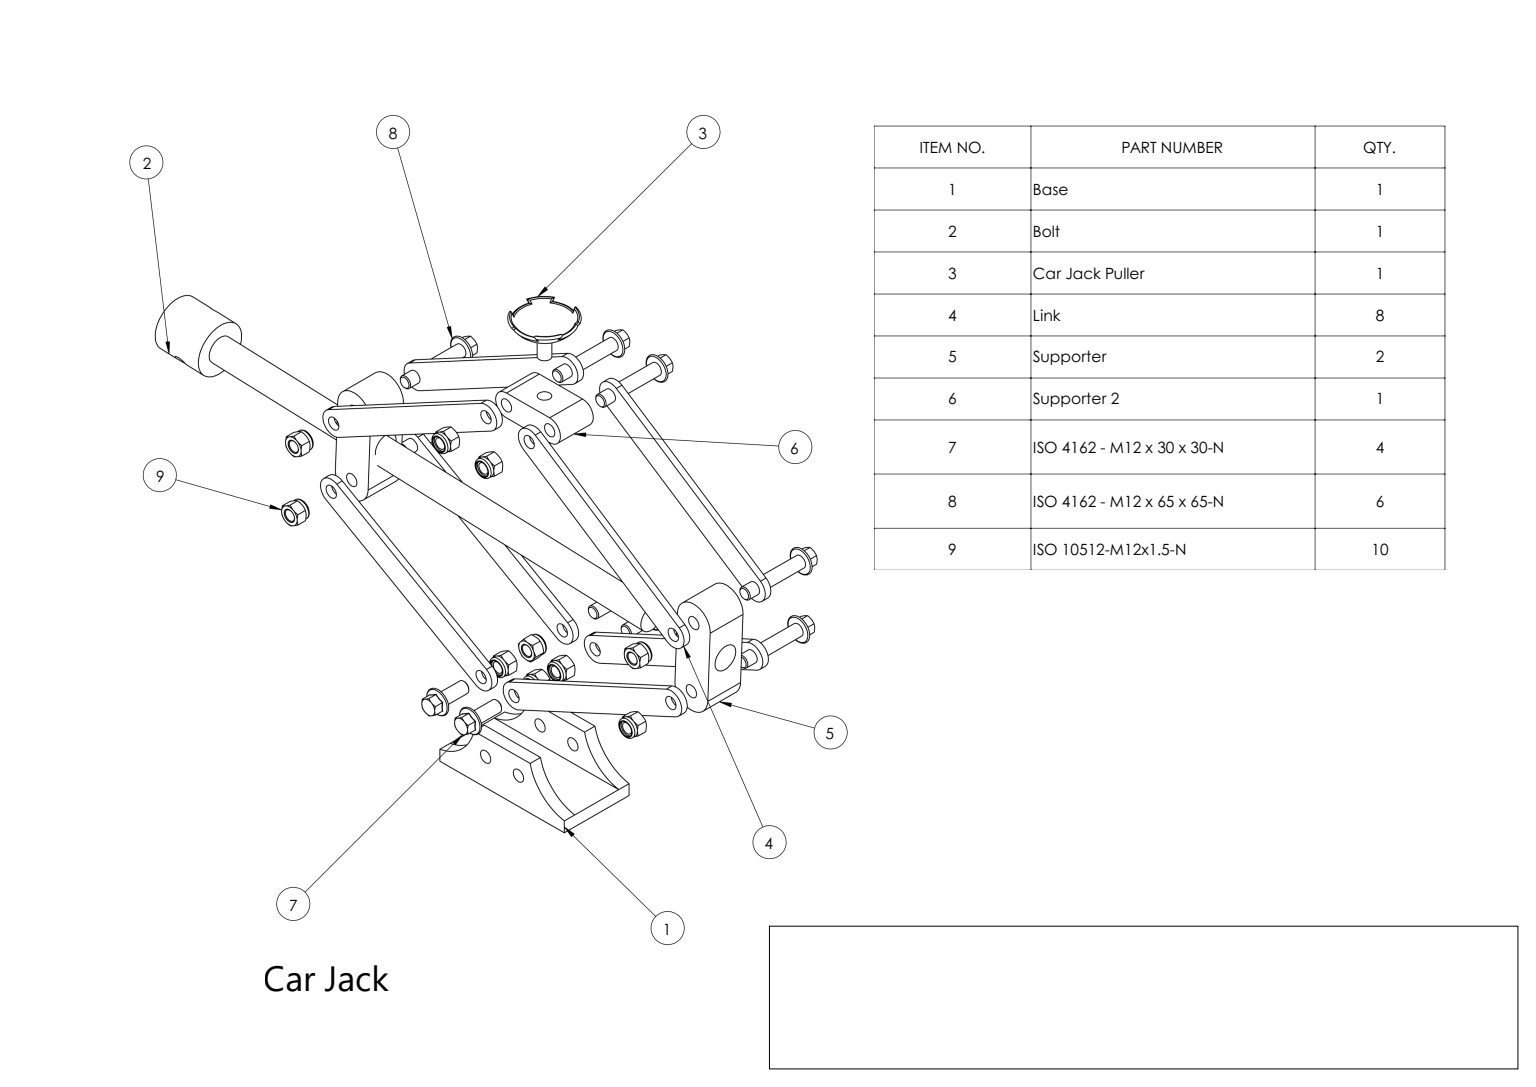
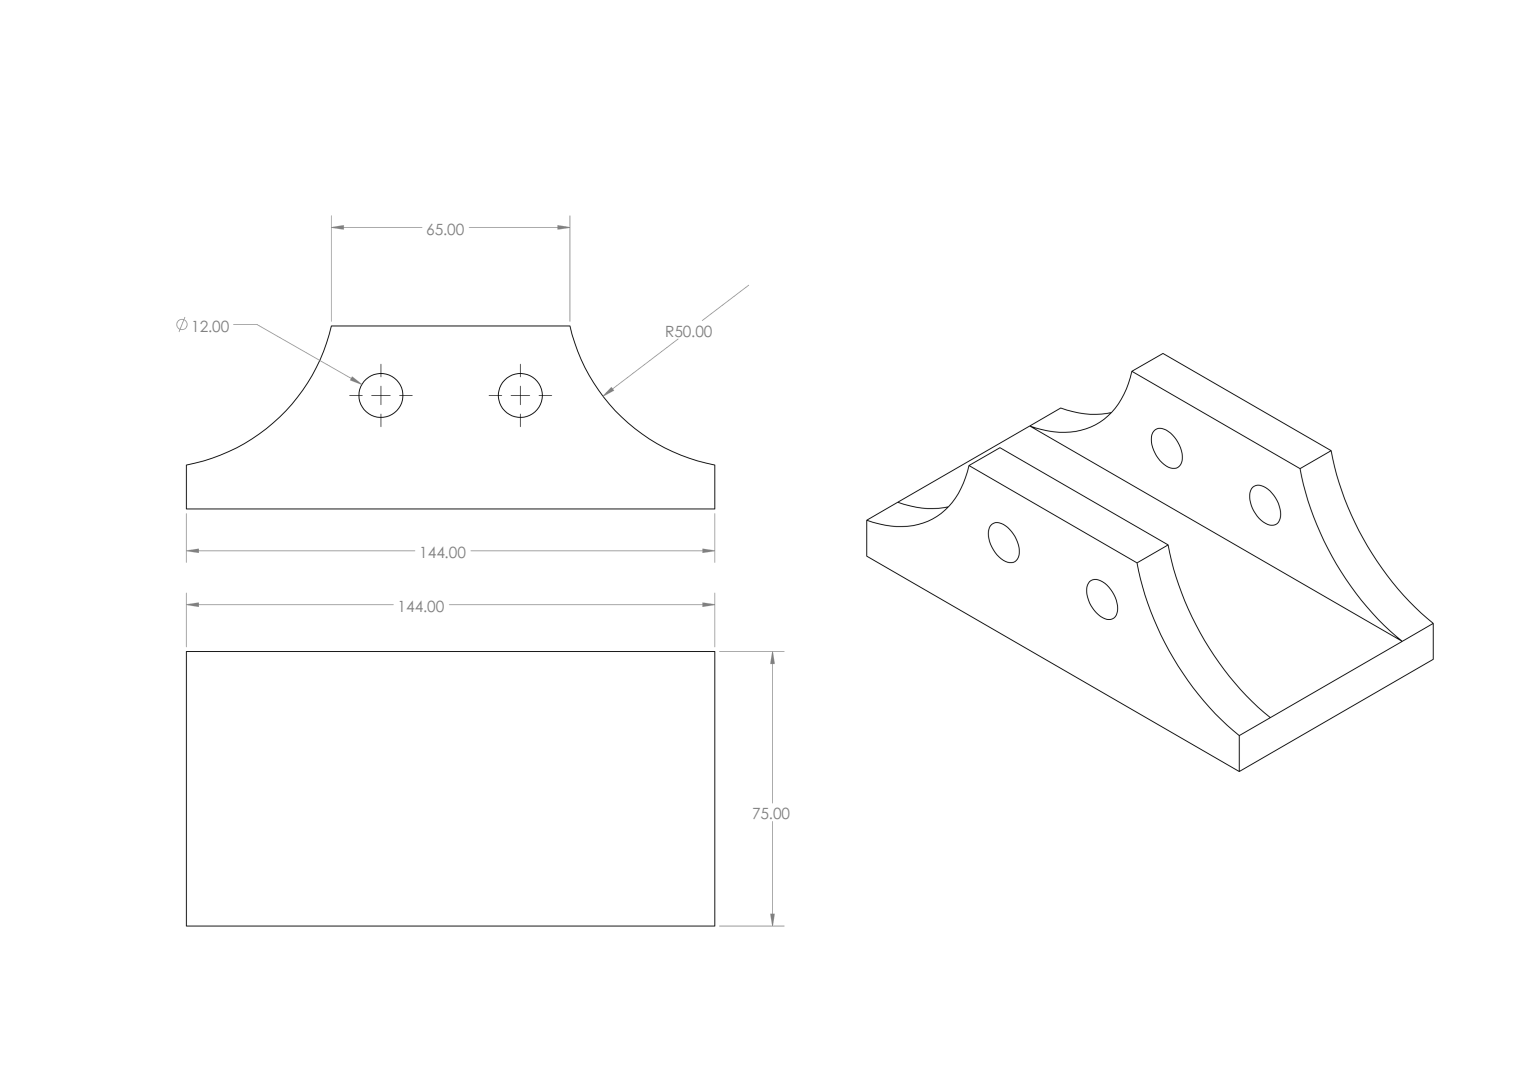
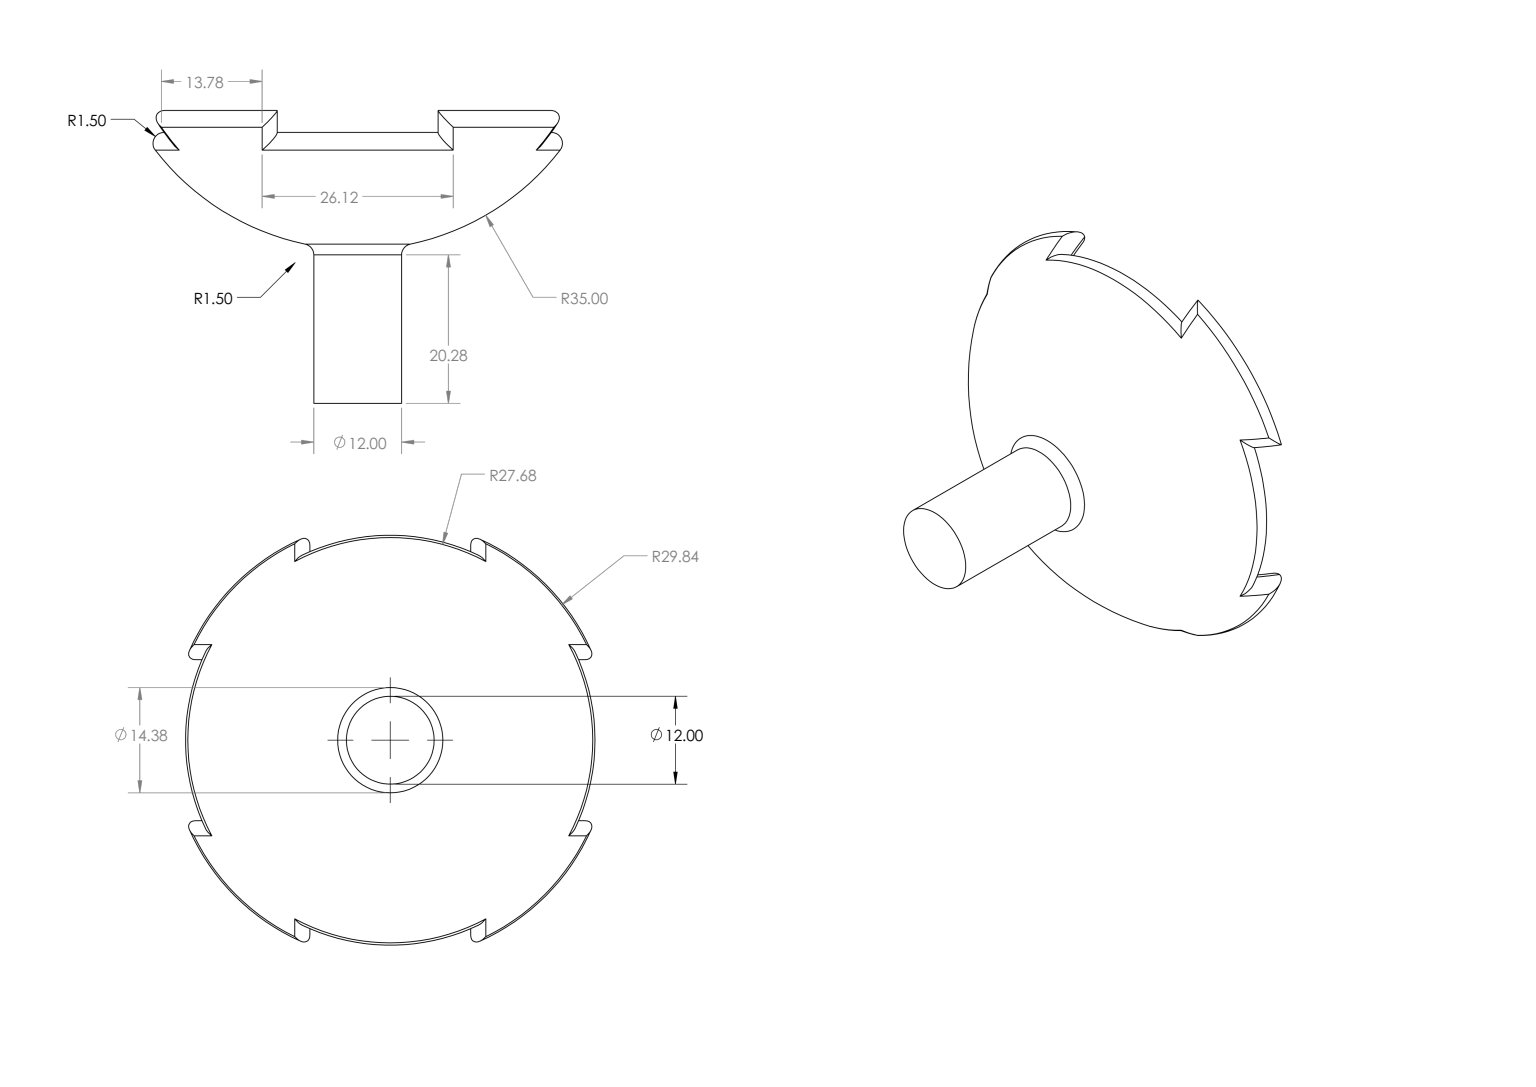
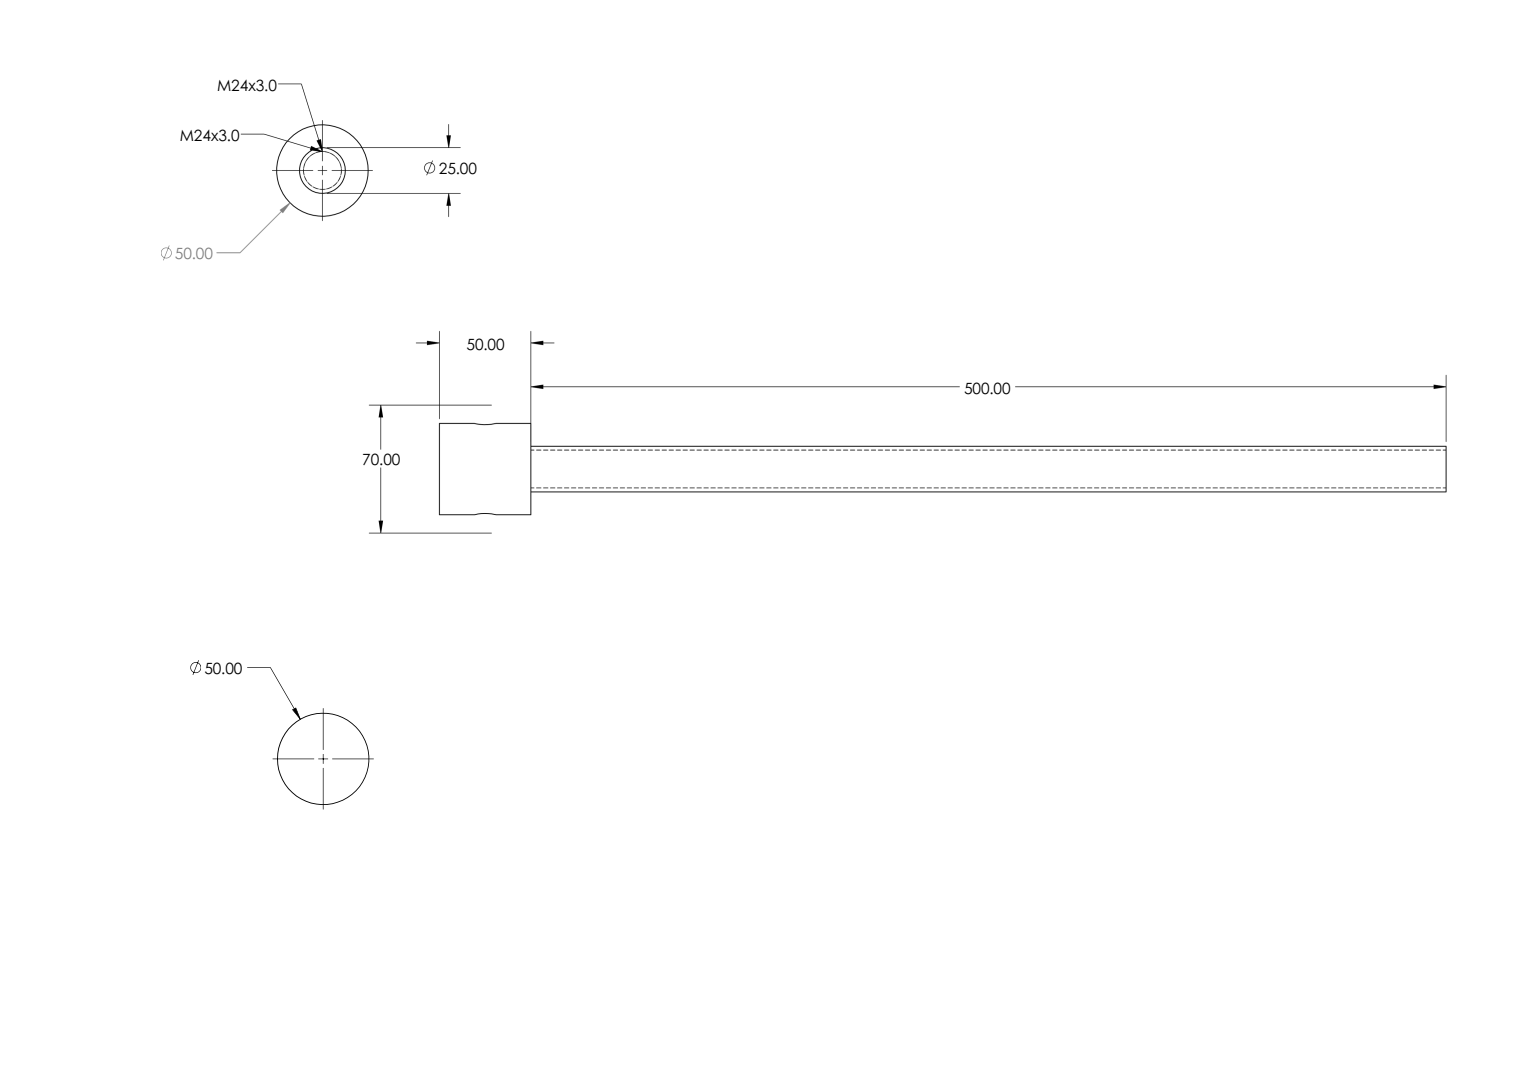
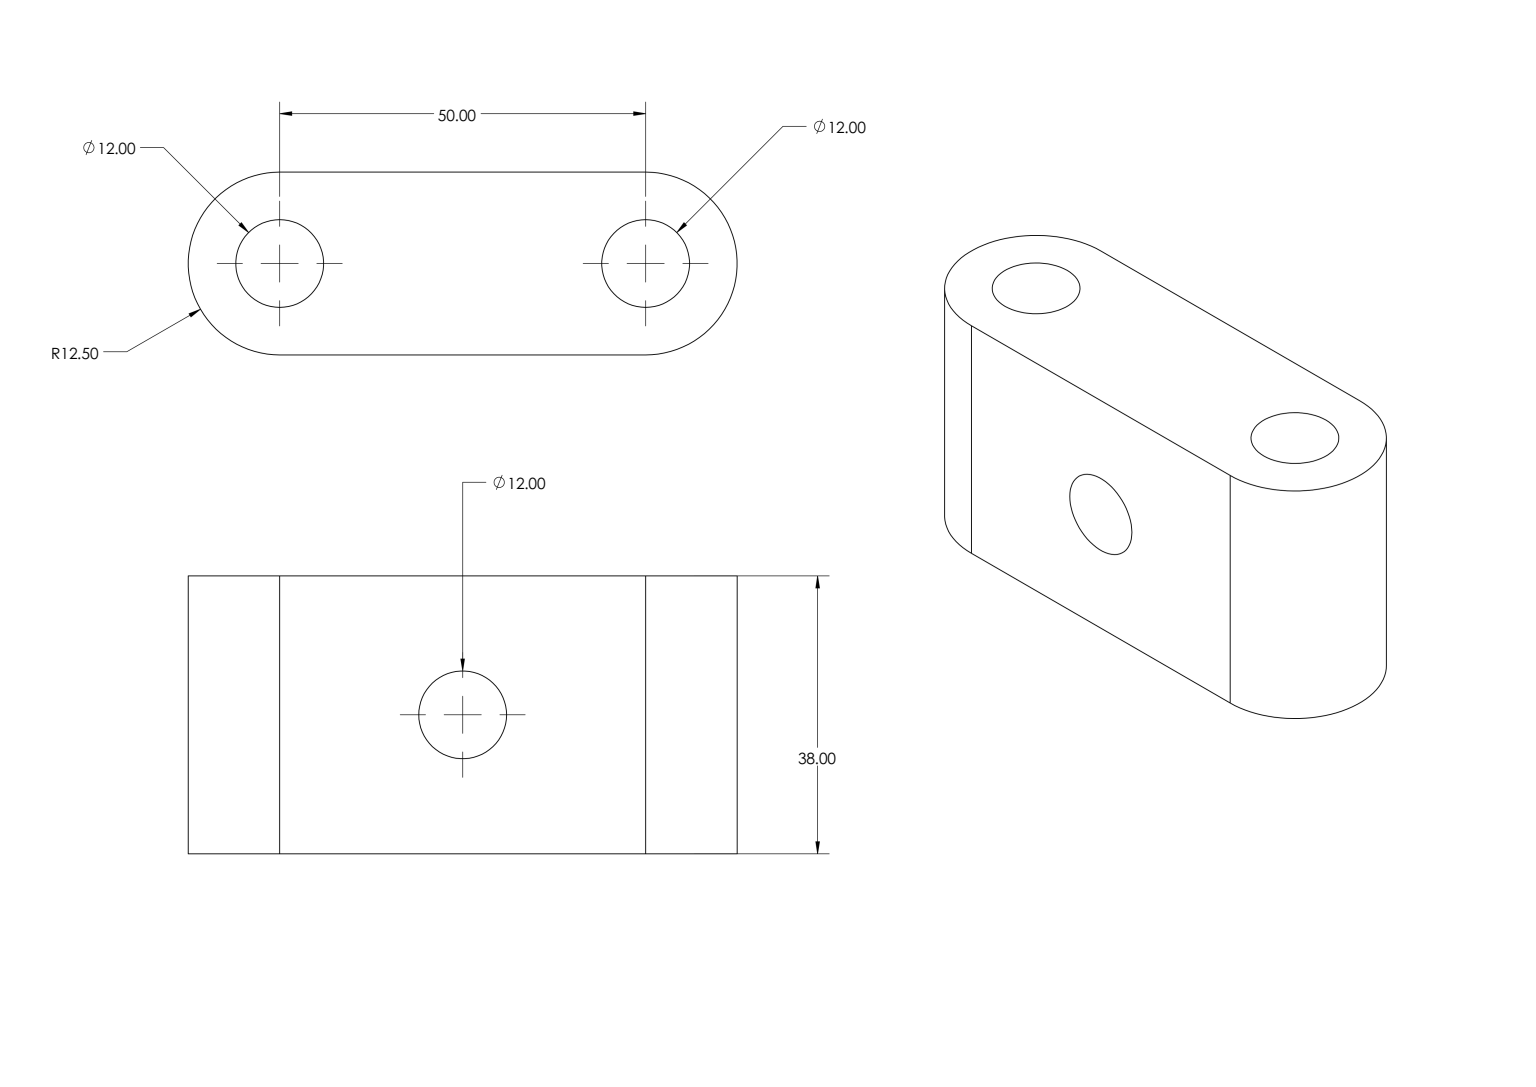
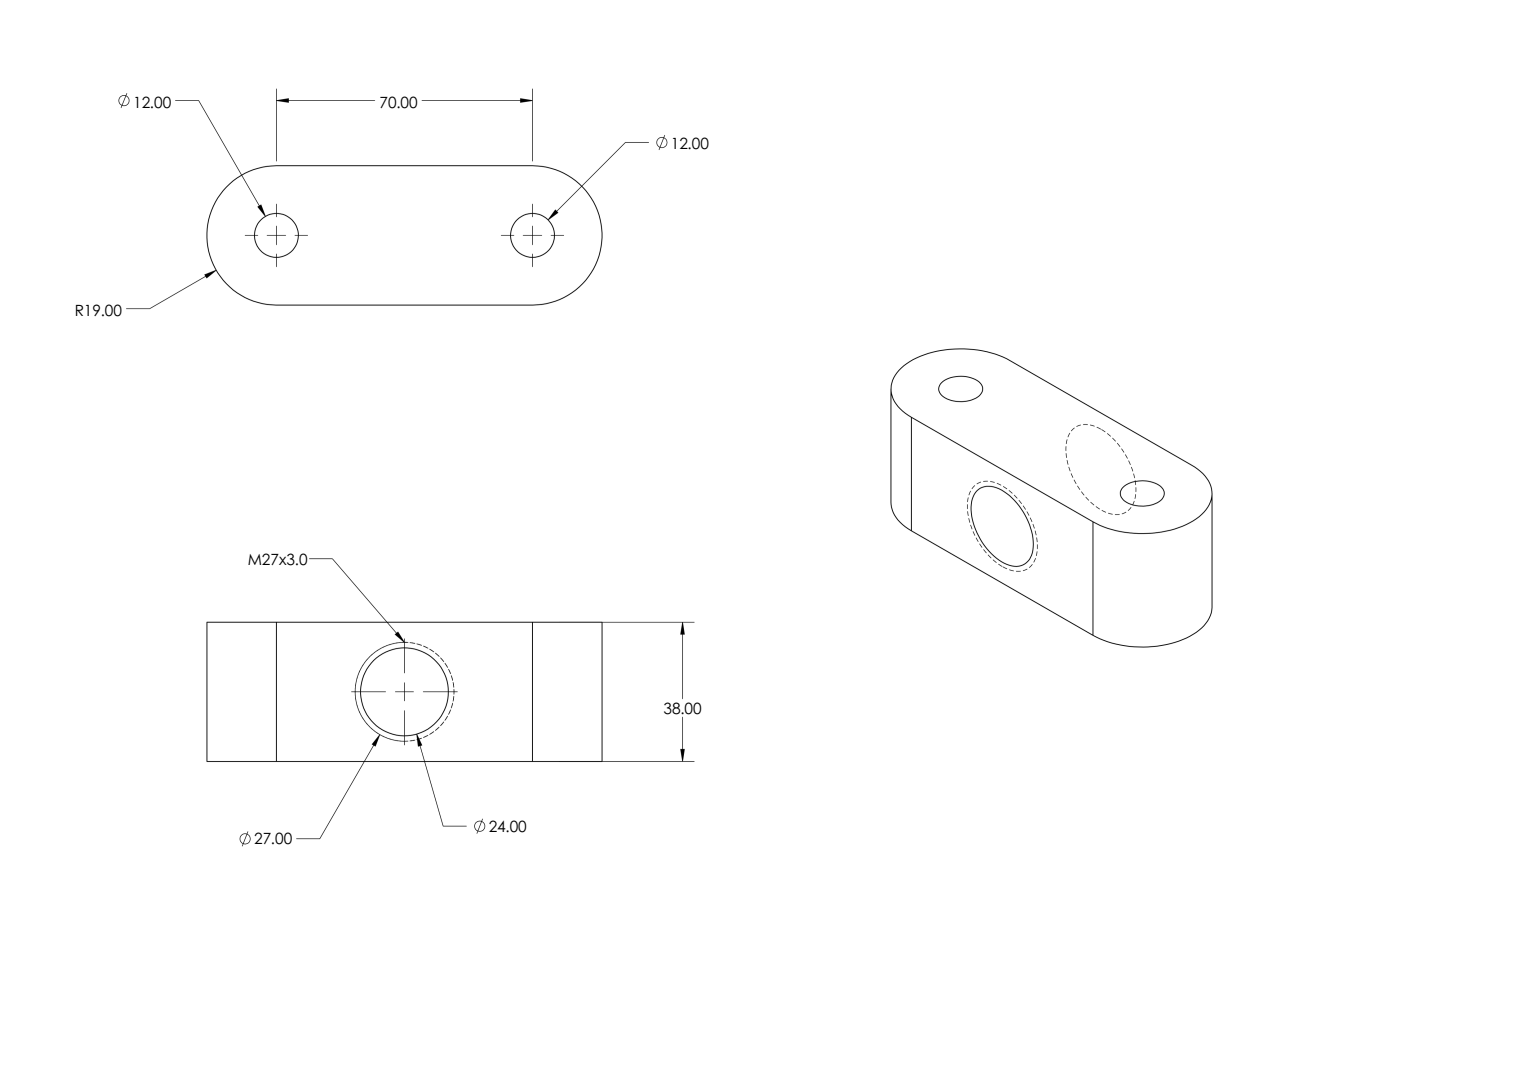
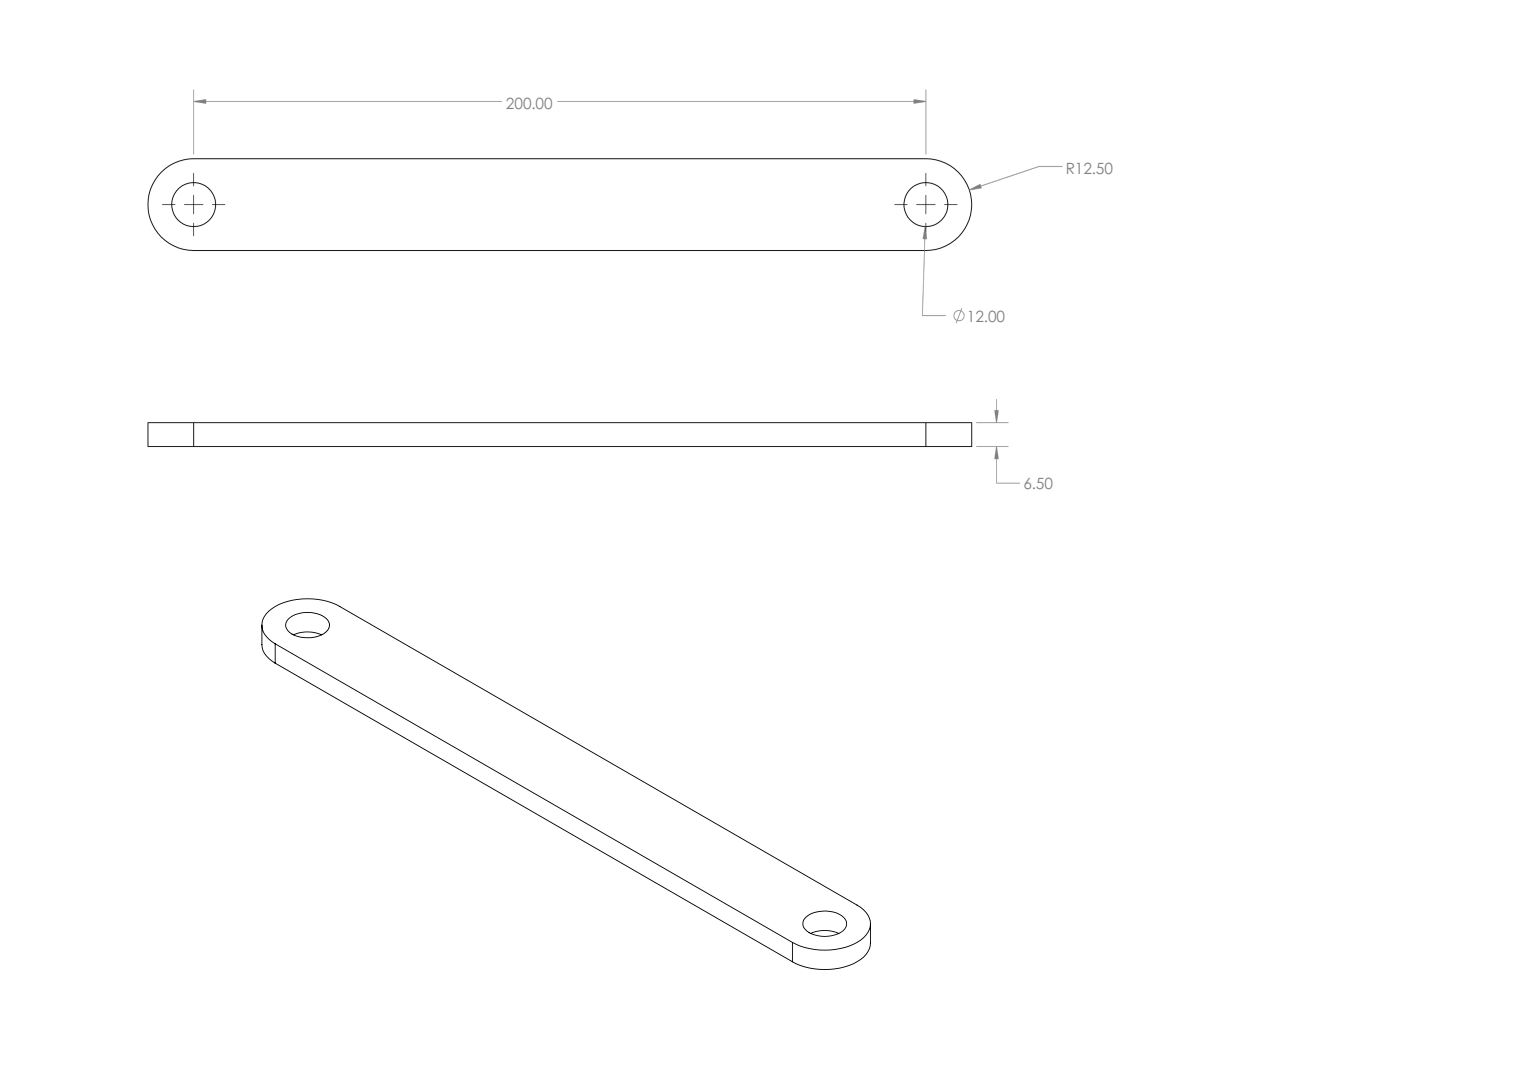
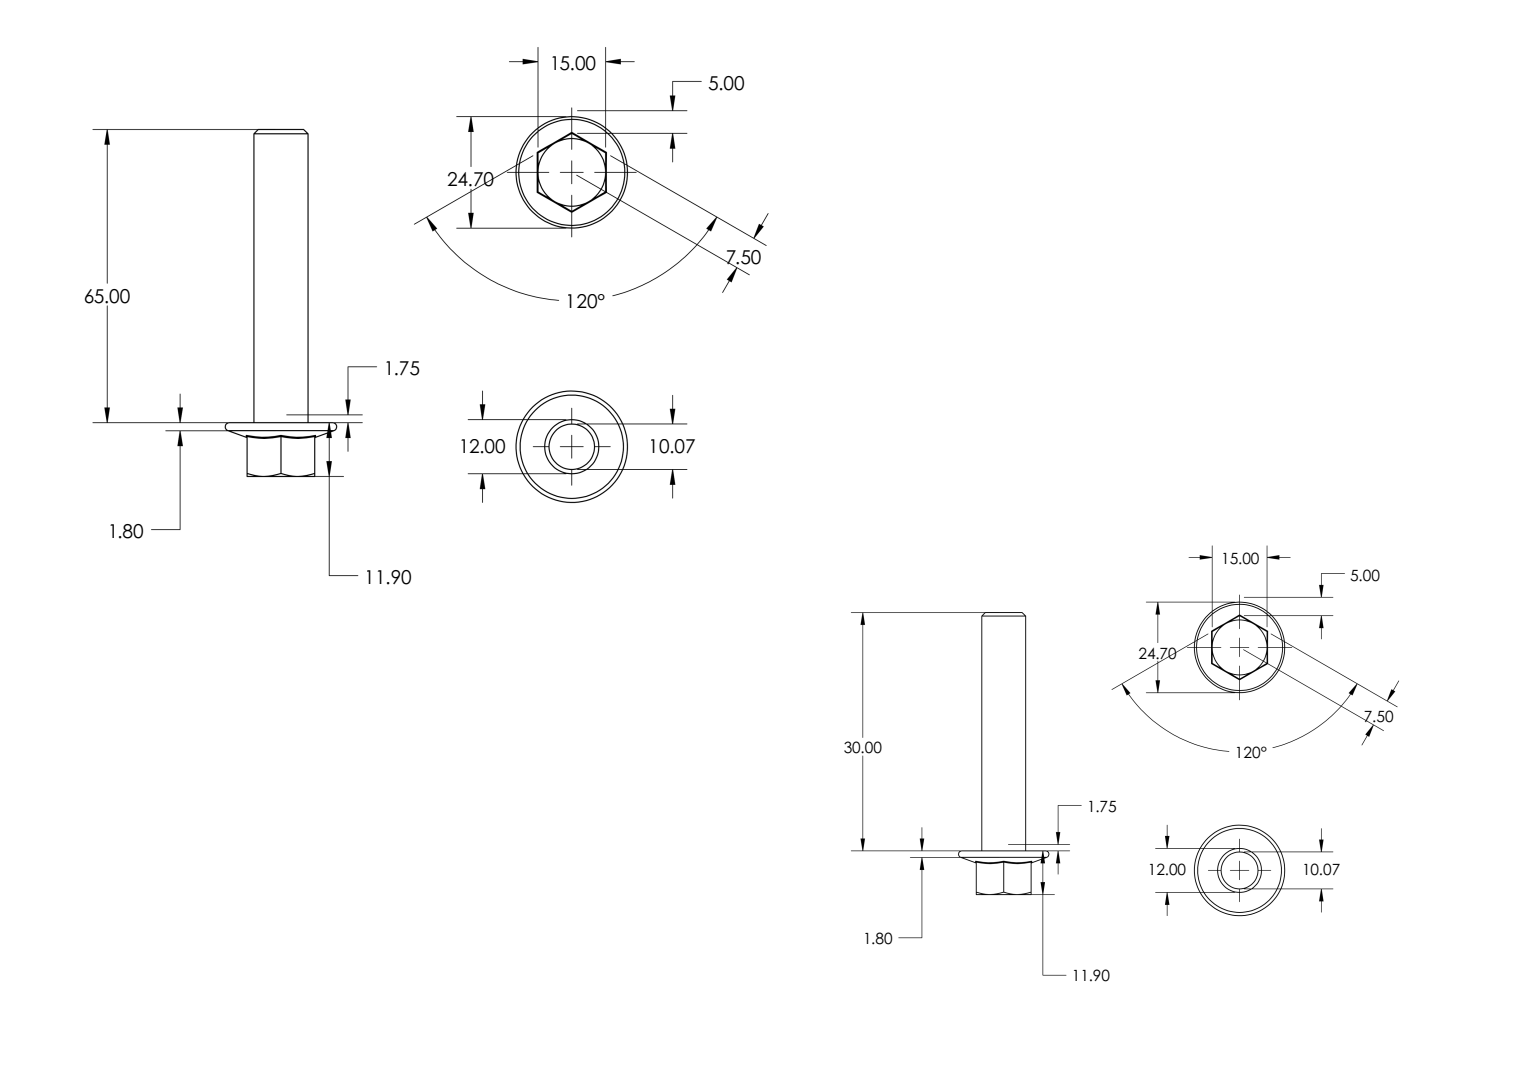
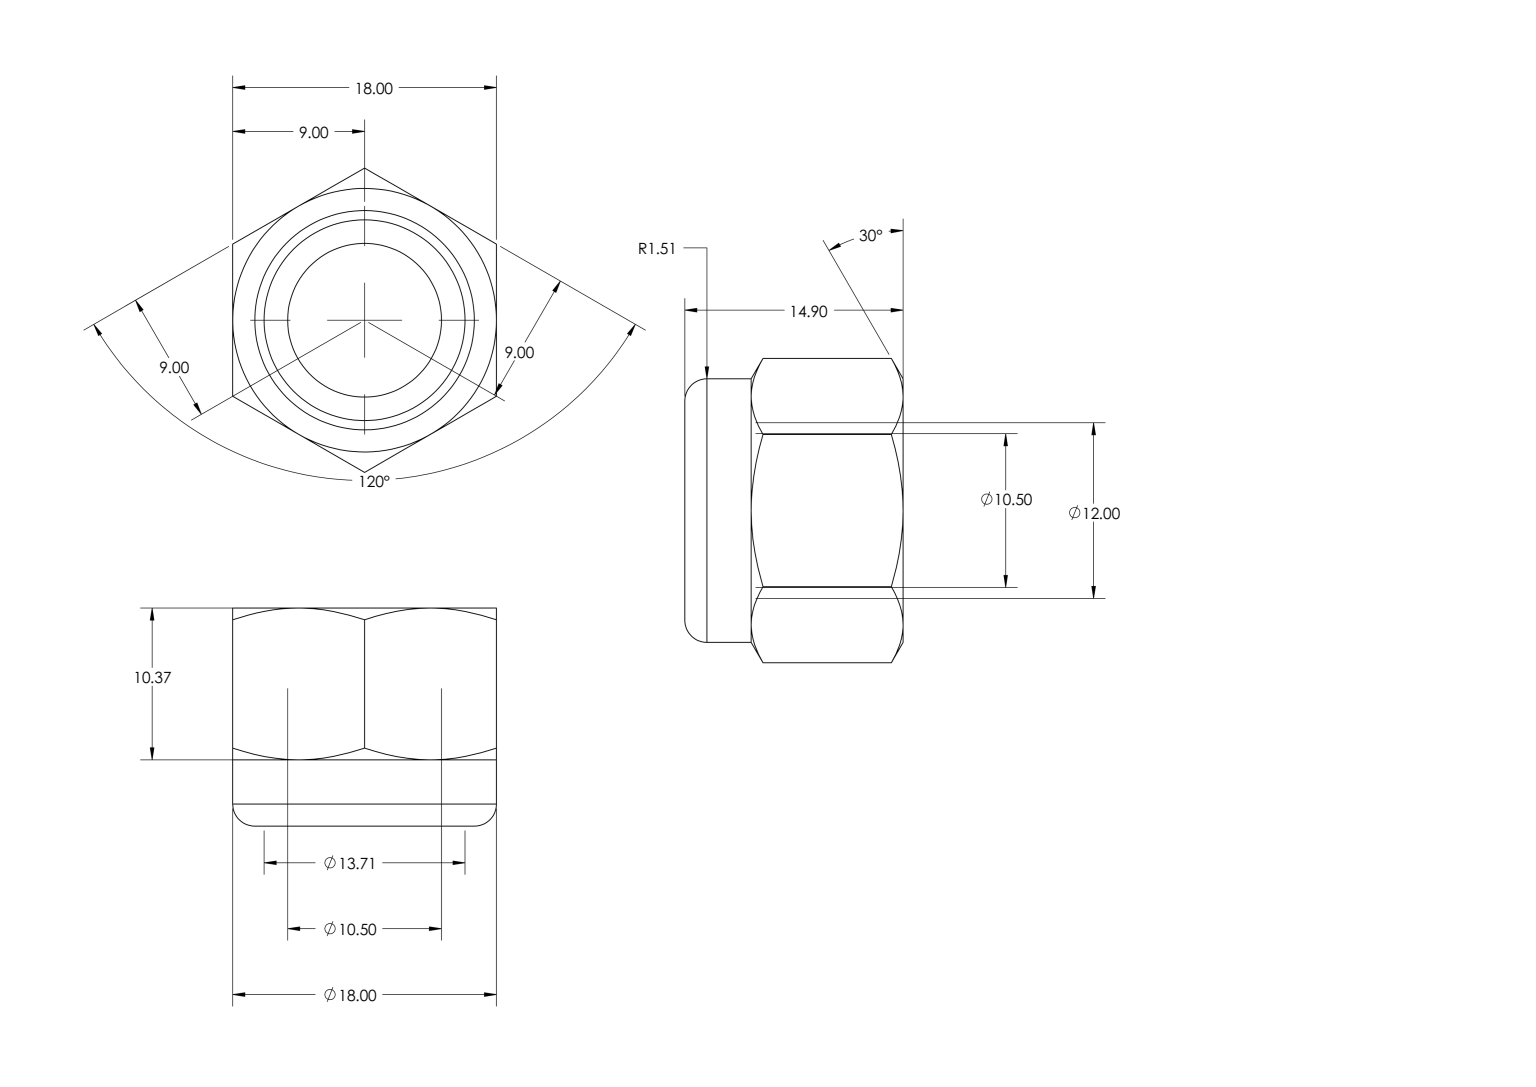
ISO-10303-21;
HEADER;
FILE_DESCRIPTION (('STEP AP214'),
    '1' );
FILE_NAME ('MAT-019',
    '2026-10-23T20:35:44',
    ( '' ),
    ( '' ),
    'SwSTEP 2.0',
    'SolidWorks 2025',
    '' );
FILE_SCHEMA (( 'AUTOMOTIVE_DESIGN' ));
ENDSEC;

DATA;
#1 = VERTEX_POINT ( 'NONE', #349 ) ;
#2 = CARTESIAN_POINT ( 'NONE',  ( 1.172031980416358365, -0.1441408498666779114, 0.9737261629585141076 ) ) ;
#3 = EDGE_CURVE ( 'NONE', #4293, #4703, #7002, .T. ) ;
#4 = CARTESIAN_POINT ( 'NONE',  ( 0.3581828924050324825, 0.3486337532542225226, 1.056976728655274672E-17 ) ) ;
#5 = ORIENTED_EDGE ( 'NONE', *, *, #5535, .F. ) ;
#6 = CARTESIAN_POINT ( 'NONE',  ( -0.3543307086614173596, -0.1713008003332314455, -0.02204270589528184790 ) ) ;
#7 = CIRCLE ( 'NONE', #3434, 0.2362204724409449064 ) ;
#8 = CARTESIAN_POINT ( 'NONE',  ( -1.023371766162646468, 0.4368380215374090825, -1.573834103987475475 ) ) ;
#9 = ADVANCED_FACE ( 'NONE', ( #4327 ), #5594, .T. ) ;
#10 = VERTEX_POINT ( 'NONE', #4360 ) ;
#11 = DIRECTION ( 'NONE',  ( -0.000000000000000000, -0.000000000000000000, 1.000000000000000000 ) ) ;
#12 = CARTESIAN_POINT ( 'NONE',  ( 0.3321019207957557895, 0.02907045490630093265, 0.2952755905511811330 ) ) ;
#13 = DIRECTION ( 'NONE',  ( -0.9237280213470682178, -0.3830490080632377725, 0.000000000000000000 ) ) ;
#14 = CIRCLE ( 'NONE', #4286, 0.4629062255509093782 ) ;
#15 =( NAMED_UNIT ( * ) PLANE_ANGLE_UNIT ( ) SI_UNIT ( $, .RADIAN. ) );
#16 = CARTESIAN_POINT ( 'NONE',  ( -0.4330708661417322913, -0.9666437042230143772, -1.454455828411337359 ) ) ;
#17 = CARTESIAN_POINT ( 'NONE',  ( 0.4330708661417324024, 0.000000000000000000, 0.000000000000000000 ) ) ;
#18 = VERTEX_POINT ( 'NONE', #5013 ) ;
#19 = FACE_OUTER_BOUND ( 'NONE', #4746, .T. ) ;
#20 = AXIS2_PLACEMENT_3D ( 'NONE', #1580, #1013, #4418 ) ;
#21 = ORIENTED_EDGE ( 'NONE', *, *, #1765, .T. ) ;
#22 = CIRCLE ( 'NONE', #2939, 0.4921259842519685179 ) ;
#23 = SHAPE_REPRESENTATION_RELATIONSHIP ( 'NONE' , 'NONE' ,  #2912, #3774 ) ;
#24 = CIRCLE ( 'NONE', #5042, 0.2362204724409449619 ) ;
#25 = DIRECTION ( 'NONE',  ( 0.000000000000000000, 0.000000000000000000, -1.000000000000000000 ) ) ;
#26 = TOROIDAL_SURFACE ( 'NONE', #1116, 1.223643328182681289, 0.05905511811023622659 ) ;
#27 = DIRECTION ( 'NONE',  ( -0.000000000000000000, 1.000000000000000000, 0.000000000000000000 ) ) ;
#28 = AXIS2_PLACEMENT_3D ( 'NONE', #7517, #513, #2824 ) ;
#29 =( REPRESENTATION_RELATIONSHIP ('NONE','NONE', #303, #1552 ) REPRESENTATION_RELATIONSHIP_WITH_TRANSFORMATION ( #2886 )SHAPE_REPRESENTATION_RELATIONSHIP( ) );
#30 = CARTESIAN_POINT ( 'NONE',  ( 0.3527008206095850751, 0.1709223649093223329, 0.2960462201727743214 ) ) ;
#31 = CARTESIAN_POINT ( 'NONE',  ( 0.3543307086614173596, -0.2045729300278204543, -0.03164754241312491001 ) ) ;
#32 = CARTESIAN_POINT ( 'NONE',  ( 0.000000000000000000, -0.2557161625347750822, -0.1476377952755907330 ) ) ;
#33 = CARTESIAN_POINT ( 'NONE',  ( -0.4330708661417322913, 0.9666437042230143772, -1.454455828411337359 ) ) ;
#34 = VERTEX_POINT ( 'NONE', #3752 ) ;
#35 = CIRCLE ( 'NONE', #6758, 1.377952755905511806 ) ;
#36 = CARTESIAN_POINT ( 'NONE',  ( -0.4330708661417317917, -1.051607547633158557, -1.573502280244650997 ) ) ;
#37 = ORIENTED_EDGE ( 'NONE', *, *, #488, .F. ) ;
#38 = CARTESIAN_POINT ( 'NONE',  ( 0.8794895096619267383, -0.2118599820681134061, 0.9611874069187010816 ) ) ;
#39 = ADVANCED_FACE ( 'NONE', ( #5518 ), #2011, .T. ) ;
#40 = DIRECTION ( 'NONE',  ( 1.000000000000000000, 0.000000000000000000, 0.000000000000000000 ) ) ;
#41 = ORIENTED_EDGE ( 'NONE', *, *, #1877, .F. ) ;
#42 = CARTESIAN_POINT ( 'NONE',  ( 0.4637694296357178780, 0.9984400756355444884, -1.410742812766313969 ) ) ;
#43 = DIRECTION ( 'NONE',  ( 1.000000000000000000, 0.000000000000000000, 0.000000000000000000 ) ) ;
#44 = ORIENTED_EDGE ( 'NONE', *, *, #3935, .F. ) ;
#45 = VECTOR ( 'NONE', #7259, 39.37007874015748143 ) ;
#46 = CARTESIAN_POINT ( 'NONE',  ( 0.000000000000000000, 2.957312202238506242E-17, 0.2952755905511810774 ) ) ;
#47 = CARTESIAN_POINT ( 'NONE',  ( -4.923936545553797639E-15, 0.4700904924197870649, -2.204724409448822975 ) ) ;
#48 = SHAPE_DEFINITION_REPRESENTATION ( #1283, #303 ) ;
#49 = EDGE_CURVE ( 'NONE', #4478, #2222, #5824, .T. ) ;
#50 = PRESENTATION_STYLE_ASSIGNMENT (( #4751 ) ) ;
#51 = EDGE_CURVE ( 'NONE', #5178, #931, #7181, .T. ) ;
#52 = DIRECTION ( 'NONE',  ( -1.000000000000000000, -0.000000000000000000, -0.000000000000000000 ) ) ;
#53 = TOROIDAL_SURFACE ( 'NONE', #1389, 1.223643328182681289, 0.05905511811023622659 ) ;
#54 = CARTESIAN_POINT ( 'NONE',  ( -1.051607547633157225, -0.4330708661417354555, -1.573502280244651441 ) ) ;
#55 = CARTESIAN_POINT ( 'NONE',  ( 0.3336175750056032396, 0.2841290694830835850, -0.09842519685039363697 ) ) ;
#56 = ORIENTED_EDGE ( 'NONE', *, *, #571, .F. ) ;
#57 = LENGTH_MEASURE_WITH_UNIT ( LENGTH_MEASURE( 0.02539999999999999897 ), #5956 );
#58 = CARTESIAN_POINT ( 'NONE',  ( 0.9346848099469073912, -0.4388997119412443304, -1.455943619906241215 ) ) ;
#59 = CARTESIAN_POINT ( 'NONE',  ( 0.000000000000000000, 0.000000000000000000, -1.515748031496062964 ) ) ;
#60 = CARTESIAN_POINT ( 'NONE',  ( 0.000000000000000000, 1.496062992125984259, -0.2362204724409449341 ) ) ;
#61 = CARTESIAN_POINT ( 'NONE',  ( 2.892866454678787531E-17, 0.000000000000000000, 0.2362204724409449341 ) ) ;
#62 = CARTESIAN_POINT ( 'NONE',  ( 0.000000000000000000, 0.000000000000000000, 0.000000000000000000 ) ) ;
#63 = PRODUCT_DEFINITION_CONTEXT ( 'detailed design', #3952, 'design' ) ;
#64 = DIRECTION ( 'NONE',  ( 0.000000000000000000, 1.000000000000000000, 0.000000000000000000 ) ) ;
#65 = CARTESIAN_POINT ( 'NONE',  ( -0.5073702590888615749, 0.9696319393318632018, -1.367288630523146420 ) ) ;
#66 = PLANE ( 'NONE',  #3064 ) ;
#67 = CARTESIAN_POINT ( 'NONE',  ( 1.048552902599916292, 0.4330708661417427274, -1.573978973432617279 ) ) ;
#68 = PLANE ( 'NONE',  #1789 ) ;
#69 = CARTESIAN_POINT ( 'NONE',  ( 0.01841426102874288775, 0.1429077274040485568, 0.2952755905511811330 ) ) ;
#70 = DIRECTION ( 'NONE',  ( -0.000000000000000000, -1.000000000000000000, -0.000000000000000000 ) ) ;
#71 = ORIENTED_EDGE ( 'NONE', *, *, #7518, .T. ) ;
#72 = PRODUCT_DEFINITION_SHAPE ( 'NONE', 'NONE',  #5982 ) ;
#73 = CARTESIAN_POINT ( 'NONE',  ( -0.4348450093584657061, -1.063161251382699124, -1.569784523562343992 ) ) ;
#74 = CARTESIAN_POINT ( 'NONE',  ( 0.3528971332113848836, -0.3341112492250008503, 0.02492269209175877395 ) ) ;
#75 = VERTEX_POINT ( 'NONE', #2557 ) ;
#76 = ORIENTED_EDGE ( 'NONE', *, *, #2854, .T. ) ;
#77 = CARTESIAN_POINT ( 'NONE',  ( 0.3581828924050323715, 0.1743168766271109560, 0.3019256869348722616 ) ) ;
#78 = AXIS2_PLACEMENT_3D ( 'NONE', #5698, #7313, #7465 ) ;
#79 = DIRECTION ( 'NONE',  ( -1.000000000000000000, -0.000000000000000000, -0.000000000000000000 ) ) ;
#80 = ORIENTED_EDGE ( 'NONE', *, *, #4669, .F. ) ;
#81 = CARTESIAN_POINT ( 'NONE',  ( 0.4999746636856467474, 0.9773775067402665773, -1.373988502838978665 ) ) ;
#82 = ORIENTED_EDGE ( 'NONE', *, *, #3467, .F. ) ;
#83 = EDGE_CURVE ( 'NONE', #5632, #7112, #5799, .T. ) ;
#84 = CYLINDRICAL_SURFACE ( 'NONE', #4175, 0.2362204724409449341 ) ;
#85 = CARTESIAN_POINT ( 'NONE',  ( 0.3337350301074833991, 0.05917206666036364110, 0.2952755905511810774 ) ) ;
#86 = CARTESIAN_POINT ( 'NONE',  ( 0.000000000000000000, 0.000000000000000000, 0.000000000000000000 ) ) ;
#87 = B_SPLINE_CURVE_WITH_KNOTS ( 'NONE', 3,
 ( #5029, #2125, #4375, #2046, #3150, #6743, #5497, #6139, #1530 ),
 .UNSPECIFIED., .F., .F.,
 ( 4, 2, 1, 2, 4 ),
 ( 0.000000000000000000, 0.002165063509461097064, 0.004330127018922194128, 0.006495190528383291625, 0.008660254037844388256 ),
 .UNSPECIFIED. ) ;
#88 = CARTESIAN_POINT ( 'NONE',  ( 0.000000000000000000, 0.000000000000000000, -0.4082677165354330340 ) ) ;
#89 = EDGE_LOOP ( 'NONE', ( #2667, #4029, #6739, #4168 ) ) ;
#90 = VECTOR ( 'NONE', #7074, 39.37007874015748143 ) ;
#91 = LINE ( 'NONE', #2420, #7062 ) ;
#92 = ORIENTED_EDGE ( 'NONE', *, *, #6917, .F. ) ;
#93 = FACE_OUTER_BOUND ( 'NONE', #3298, .T. ) ;
#94 = B_SPLINE_CURVE_WITH_KNOTS ( 'NONE', 3,
 ( #4855, #1250, #5355, #240, #5937, #4783, #5402, #7182 ),
 .UNSPECIFIED., .F., .F.,
 ( 4, 2, 2, 4 ),
 ( 0.005257893453559878486, 0.006567392922673220834, 0.007876892391786563183, 0.01049589133001324615 ),
 .UNSPECIFIED. ) ;
#95 = EDGE_CURVE ( 'NONE', #3796, #3264, #4939, .T. ) ;
#96 = VERTEX_POINT ( 'NONE', #2710 ) ;
#97 = EDGE_CURVE ( 'NONE', #6349, #6629, #5465, .T. ) ;
#98 = AXIS2_PLACEMENT_3D ( 'NONE', #2181, #4591, #4516 ) ;
#99 = EDGE_CURVE ( 'NONE', #6172, #3346, #1437, .T. ) ;
#100 = CARTESIAN_POINT ( 'NONE',  ( -0.4437902010346558290, 0.9221077491748241872, -1.453484313640523107 ) ) ;
#101 = CARTESIAN_POINT ( 'NONE',  ( 2.755905511811024056, 1.496062992125984259, -0.7480314960629921295 ) ) ;
#102 = DIRECTION ( 'NONE',  ( -1.000000000000000000, 0.000000000000000000, 0.000000000000000000 ) ) ;
#103 = VECTOR ( 'NONE', #1652, 39.37007874015748143 ) ;
#104 = CARTESIAN_POINT ( 'NONE',  ( 0.3411144883932946681, 0.06120045565151401717, -0.3014953316451452481 ) ) ;
#105 = FACE_BOUND ( 'NONE', #1838, .T. ) ;
#106 = CARTESIAN_POINT ( 'NONE',  ( -0.4349192958999751890, 0.9810556462971158354, -1.448591228719268820 ) ) ;
#107 = CARTESIAN_POINT ( 'NONE',  ( 1.649606299212598381, 0.000000000000000000, 0.000000000000000000 ) ) ;
#108 = AXIS2_PLACEMENT_3D ( 'NONE', #6313, #3367, #512 ) ;
#109 = ITEM_DEFINED_TRANSFORMATION ( 'NONE', 'NONE', #1772,  #5166 ) ;
#110 = DIRECTION ( 'NONE',  ( -1.000000000000000000, 0.000000000000000000, 0.000000000000000000 ) ) ;
#111 = CYLINDRICAL_SURFACE ( 'NONE', #3021, 0.2362204724409448231 ) ;
#112 = FACE_OUTER_BOUND ( 'NONE', #858, .T. ) ;
#113 = CARTESIAN_POINT ( 'NONE',  ( -0.7480314960629922405, 1.220472440944881942, 0.000000000000000000 ) ) ;
#114 = ORIENTED_EDGE ( 'NONE', *, *, #6223, .T. ) ;
#115 = B_SPLINE_CURVE_WITH_KNOTS ( 'NONE', 3,
 ( #6451, #6987, #1865, #683, #4728, #5964, #4691, #7061, #719 ),
 .UNSPECIFIED., .F., .F.,
 ( 4, 2, 1, 2, 4 ),
 ( 0.000000000000000000, 0.002165063509461098365, 0.004330127018922196730, 0.006495190528383293360, 0.008660254037844391725 ),
 .UNSPECIFIED. ) ;
#116 = CARTESIAN_POINT ( 'NONE',  ( -0.5141614760841455301, -1.056523642887403414, -1.484898342931014081 ) ) ;
#117 = B_SPLINE_CURVE_WITH_KNOTS ( 'NONE', 3,
 ( #3701, #1901, #4841, #4348, #5547, #6644, #2544, #3159, #6569, #5505, #6716, #789, #6606, #304, #7249, #1393, #4232, #1353 ),
 .UNSPECIFIED., .F., .F.,
 ( 4, 2, 2, 2, 2, 2, 2, 2, 4 ),
 ( 0.000000000000000000, 0.0002327816859446662134, 0.0004655633718893324269, 0.0009311267437786553127, 0.001396690115667978144, 0.001862253487557301085, 0.002327816859446624025, 0.002793380231335946748, 0.003724506975114579184 ),
 .UNSPECIFIED. ) ;
#118 = AXIS2_PLACEMENT_3D ( 'NONE', #1172, #3453, #43 ) ;
#119 = EDGE_LOOP ( 'NONE', ( #4224, #2865, #7199, #7516, #208 ) ) ;
#120 = ORIENTED_EDGE ( 'NONE', *, *, #5116, .T. ) ;
#121 = CARTESIAN_POINT ( 'NONE',  ( 0.3410249605999410294, 1.062103031354818709E-12, 0.3014927230551906479 ) ) ;
#122 = CIRCLE ( 'NONE', #5251, 1.968503937007874072 ) ;
#123 = LINE ( 'NONE', #695, #2284 ) ;
#124 = ORIENTED_EDGE ( 'NONE', *, *, #6507, .T. ) ;
#125 = LINE ( 'NONE', #7263, #284 ) ;
#126 = CARTESIAN_POINT ( 'NONE',  ( 0.3997746709170348356, 0.000000000000000000, 0.000000000000000000 ) ) ;
#127 = ORIENTED_EDGE ( 'NONE', *, *, #95, .F. ) ;
#128 = ORIENTED_EDGE ( 'NONE', *, *, #6591, .F. ) ;
#129 = CARTESIAN_POINT ( 'NONE',  ( 2.834645669291338876, 0.4724409448818890911, 0.4724409448818898127 ) ) ;
#130 = CYLINDRICAL_SURFACE ( 'NONE', #5377, 0.2362204724409448231 ) ;
#131 = CARTESIAN_POINT ( 'NONE',  ( 0.3543307086614173040, 0.2045729300278205931, -0.3766201741223081378 ) ) ;
#132 = ORIENTED_EDGE ( 'NONE', *, *, #2423, .T. ) ;
#133 = CARTESIAN_POINT ( 'NONE',  ( 1.078368654584408670, -0.4878048847236703955, -1.510181419419386772 ) ) ;
#134 = EDGE_CURVE ( 'NONE', #2064, #5110, #3716, .T. ) ;
#135 = VERTEX_POINT ( 'NONE', #1514 ) ;
#136 = CARTESIAN_POINT ( 'NONE',  ( 0.3528850351813196395, -0.1886720902358828833, 0.2768301761068310274 ) ) ;
#137 =( REPRESENTATION_RELATIONSHIP ('NONE','NONE', #303, #5265 ) REPRESENTATION_RELATIONSHIP_WITH_TRANSFORMATION ( #1320 )SHAPE_REPRESENTATION_RELATIONSHIP( ) );
#138 = CARTESIAN_POINT ( 'NONE',  ( 0.000000000000000000, 0.000000000000000000, 0.000000000000000000 ) ) ;
#139 = VERTEX_POINT ( 'NONE', #316 ) ;
#140 = CARTESIAN_POINT ( 'NONE',  ( 15.64880248481180303, 40.22106072789451048, 53.38200498105501168 ) ) ;
#141 = PRODUCT ( 'Bolt', 'Bolt', '', ( #5415 ) ) ;
#142 = CARTESIAN_POINT ( 'NONE',  ( 1.068462032678259234E-16, -0.2629500981735136689, -0.1351082512106133171 ) ) ;
#143 = CARTESIAN_POINT ( 'NONE',  ( 0.7480314960629923515, 1.205359478595430764E-16, -0.9842519685039370358 ) ) ;
#144 = EDGE_CURVE ( 'NONE', #1513, #5818, #3845, .T. ) ;
#145 = EDGE_CURVE ( 'NONE', #322, #18, #7008, .T. ) ;
#146 = CIRCLE ( 'NONE', #633, 1.043121362164705745 ) ;
#147 = CARTESIAN_POINT ( 'NONE',  ( -0.8785537298370117432, -0.4700904924197938373, -1.433776001880364470 ) ) ;
#148 = EDGE_CURVE ( 'NONE', #5183, #4410, #5219, .T. ) ;
#149 = CARTESIAN_POINT ( 'NONE',  ( 0.5141614760841460852, -0.9609181420092316461, -1.361499588670819216 ) ) ;
#150 = CARTESIAN_POINT ( 'NONE',  ( 0.3543307086614173040, -0.06891495372886455306, -0.002971448422589516563 ) ) ;
#151 = CARTESIAN_POINT ( 'NONE',  ( 1.377952755905512028, 0.7480314960629921295, 0.7480314960629921295 ) ) ;
#152 = CONTEXT_DEPENDENT_SHAPE_REPRESENTATION ( #2365, #209 ) ;
#153 = DIRECTION ( 'NONE',  ( -0.000000000000000000, -0.000000000000000000, 1.000000000000000000 ) ) ;
#154 = VECTOR ( 'NONE', #737, 39.37007874015748143 ) ;
#155 = CYLINDRICAL_SURFACE ( 'NONE', #855, 0.7480314960629921295 ) ;
#156 = ADVANCED_FACE ( 'NONE', ( #5228 ), #2856, .T. ) ;
#157 = CARTESIAN_POINT ( 'NONE',  ( 1.041228047528458989, -0.4333661275891970699, -1.574803149606299302 ) ) ;
#158 = DIRECTION ( 'NONE',  ( 1.000000000000000000, 0.000000000000000000, 0.000000000000000000 ) ) ;
#159 = CARTESIAN_POINT ( 'NONE',  ( 0.01832242175888446414, 0.1844213691142423395, 0.2711239997950803393 ) ) ;
#160 = EDGE_CURVE ( 'NONE', #5534, #5278, #5680, .T. ) ;
#161 = VERTEX_POINT ( 'NONE', #540 ) ;
#162 = CARTESIAN_POINT ( 'NONE',  ( 1.968503937007874072, 1.496062992125984259, 0.000000000000000000 ) ) ;
#163 = CARTESIAN_POINT ( 'NONE',  ( 0.3426404862726872280, -0.2904653615686530466, 0.09998168480679490988 ) ) ;
#164 = CIRCLE ( 'NONE', #5660, 0.2362204724409449619 ) ;
#165 = ORIENTED_EDGE ( 'NONE', *, *, #6591, .T. ) ;
#166 = AXIS2_PLACEMENT_3D ( 'NONE', #1159, #469, #4589 ) ;
#167 = DIRECTION ( 'NONE',  ( -0.000000000000000000, -1.000000000000000000, -0.000000000000000000 ) ) ;
#168 = CIRCLE ( 'NONE', #5420, 1.278433327952054555 ) ;
#169 = CARTESIAN_POINT ( 'NONE',  ( 0.3528850351813196951, 0.1886720902358826890, -0.2768301761068310274 ) ) ;
#170 = ORIENTED_EDGE ( 'NONE', *, *, #1680, .T. ) ;
#171 = DIRECTION ( 'NONE',  ( 0.000000000000000000, -0.000000000000000000, 1.000000000000000000 ) ) ;
#172 = ORIENTED_EDGE ( 'NONE', *, *, #5240, .T. ) ;
#173 = CIRCLE ( 'NONE', #4442, 0.2362204724409449341 ) ;
#174 = ORIENTED_EDGE ( 'NONE', *, *, #5753, .F. ) ;
#175 = CARTESIAN_POINT ( 'NONE',  ( 0.3391216574607823775, -0.1954800165277041091, -0.2519698606119756268 ) ) ;
#176 = SHAPE_DEFINITION_REPRESENTATION ( #334, #2147 ) ;
#177 = CARTESIAN_POINT ( 'NONE',  ( 0.3997746709170348356, 5.668966274263039413E-17, 0.4629062255509093782 ) ) ;
#178 = CARTESIAN_POINT ( 'NONE',  ( 0.3388543739203577765, -0.06138491293039709945, 0.2952755905511811330 ) ) ;
#179 = CARTESIAN_POINT ( 'NONE',  ( 1.080458355692619721, -0.4837911690062307035, -1.514208178040841846 ) ) ;
#180 = CARTESIAN_POINT ( 'NONE',  ( -0.4466264210910796950, -0.9159926810392101659, -1.451746030331785509 ) ) ;
#181 = CARTESIAN_POINT ( 'NONE',  ( 0.3581828924050327045, -0.3486337532542230222, -1.123169198254405176E-18 ) ) ;
#182 = ORIENTED_EDGE ( 'NONE', *, *, #5478, .F. ) ;
#183 = CARTESIAN_POINT ( 'NONE',  ( 0.3391216574607823775, -0.1954800165277041091, -0.2519698606119756268 ) ) ;
#184 = SURFACE_SIDE_STYLE ('',( #3699 ) ) ;
#185 = CARTESIAN_POINT ( 'NONE',  ( -0.9159926810392086116, -0.4466264210910828036, -1.451746030331785509 ) ) ;
#186 = FACE_OUTER_BOUND ( 'NONE', #1523, .T. ) ;
#187 = EDGE_CURVE ( 'NONE', #6581, #698, #1547, .T. ) ;
#188 = CARTESIAN_POINT ( 'NONE',  ( 0.3391892065151629887, 0.1136516277932332897, 0.2952755905511810774 ) ) ;
#189 = CARTESIAN_POINT ( 'NONE',  ( 1.084813347358858593, 0.4713815370807524219, -1.526966122205014820 ) ) ;
#190 = DIRECTION ( 'NONE',  ( -0.000000000000000000, -0.000000000000000000, -1.000000000000000000 ) ) ;
#191 = B_SPLINE_CURVE_WITH_KNOTS ( 'NONE', 3,
 ( #3189, #3844, #2647, #6068, #7236, #2009, #5539, #6708, #896, #7196, #1384, #1453, #4340, #3875, #972, #4412, #4297, #327, #4989, #7308, #2085, #1493, #6175, #930, #3260, #3299, #5650, #6636, #3380, #1719, #6358, #3962, #2195, #6932, #7494, #2869, #5212, #3419, #6326, #1574 ),
 .UNSPECIFIED., .F., .F.,
 ( 4, 2, 2, 2, 2, 2, 2, 2, 2, 2, 2, 2, 2, 2, 2, 2, 2, 2, 2, 4 ),
 ( 0.01882766236946021784, 0.02000407617178198011, 0.02118048997410373890, 0.02176869687526461830, 0.02235690377642549770, 0.02353331757874724955, 0.02470973138106900141, 0.02588614518339075327, 0.02706255898571250512, 0.02765076588687337758, 0.02823897278803425004, 0.02941538659035599496, 0.03059180039267773293, 0.03176821419499947785, 0.03235642109616034684, 0.03294462799732121583, 0.03412104179964296768, 0.03529745560196471260, 0.03647386940428645752, 0.03765028320660820244 ),
 .UNSPECIFIED. ) ;
#192 = CARTESIAN_POINT ( 'NONE',  ( 0.3997746709170348356, 0.000000000000000000, -0.4629062255509093782 ) ) ;
#193 = LINE ( 'NONE', #1323, #3033 ) ;
#194 = CARTESIAN_POINT ( 'NONE',  ( -1.678725927747302331E-16, 0.2411939993270974525, 0.1727909197870958202 ) ) ;
#195 = ORIENTED_EDGE ( 'NONE', *, *, #3184, .F. ) ;
#196 = CARTESIAN_POINT ( 'NONE',  ( -0.9609181420092336445, 0.5141614760841427545, -1.361499588670819216 ) ) ;
#197 = DIRECTION ( 'NONE',  ( -0.000000000000000000, -0.000000000000000000, 1.000000000000000000 ) ) ;
#198 = B_SPLINE_CURVE_WITH_KNOTS ( 'NONE', 3,
 ( #225, #6215, #6608, #5615, #3303, #2545 ),
 .UNSPECIFIED., .F., .F.,
 ( 4, 2, 4 ),
 ( 0.02186578511398849095, 0.02405896738650913774, 0.02625214965902978106 ),
 .UNSPECIFIED. ) ;
#199 = ORIENTED_EDGE ( 'NONE', *, *, #4211, .F. ) ;
#200 = ADVANCED_FACE ( 'NONE', ( #5743 ), #3325, .T. ) ;
#201 = ADVANCED_FACE ( 'NONE', ( #6803 ), #1631, .T. ) ;
#202 = CARTESIAN_POINT ( 'NONE',  ( 0.3465697713329959906, -0.1180955399632931530, -0.2952755905511810774 ) ) ;
#203 = DIRECTION ( 'NONE',  ( 0.000000000000000000, -0.000000000000000000, -1.000000000000000000 ) ) ;
#204 = ADVANCED_FACE ( 'NONE', ( #508 ), #6894, .T. ) ;
#205 = CARTESIAN_POINT ( 'NONE',  ( 1.649606299212598381, 0.000000000000000000, 0.1982677165354330695 ) ) ;
#206 = ORIENTED_EDGE ( 'NONE', *, *, #1251, .T. ) ;
#207 = CARTESIAN_POINT ( 'NONE',  ( 0.3322361761492156895, 0.2866471735582875047, -0.09406371265339424914 ) ) ;
#208 = ORIENTED_EDGE ( 'NONE', *, *, #4312, .F. ) ;
#209 = PRODUCT_DEFINITION_SHAPE ( 'NONE', 'NONE',  #7547 ) ;
#210 = VERTEX_POINT ( 'NONE', #5171 ) ;
#211 = CYLINDRICAL_SURFACE ( 'NONE', #635, 0.2362204724409449896 ) ;
#212 = PRODUCT_DEFINITION_FORMATION_WITH_SPECIFIED_SOURCE ( 'ANY', '', #141, .NOT_KNOWN. ) ;
#213 = APPLICATION_PROTOCOL_DEFINITION ( 'draft international standard', 'automotive_design', 1998, #673 ) ;
#214 = CARTESIAN_POINT ( 'NONE',  ( 1.968503937007874072, 0.000000000000000000, 0.000000000000000000 ) ) ;
#215 = B_SPLINE_CURVE_WITH_KNOTS ( 'NONE', 3,
 ( #4148, #5462, #5874, #221, #2542, #2507, #3617, #677, #5336, #2427, #1312, #7093, #1857, #4839, #714, #747, #3037, #5380 ),
 .UNSPECIFIED., .F., .F.,
 ( 4, 2, 2, 2, 2, 2, 2, 2, 4 ),
 ( 0.000000000000000000, 0.0002327816859446665387, 0.0004655633718893330774, 0.0009311267437786566138, 0.001396690115667980096, 0.001862253487557303687, 0.002327816859446627060, 0.002793380231335950651, 0.003724506975114584388 ),
 .UNSPECIFIED. ) ;
#216 = CARTESIAN_POINT ( 'NONE',  ( 0.3387177083556158763, 0.2701412011613934516, 0.1226528954731279514 ) ) ;
#217 = ORIENTED_EDGE ( 'NONE', *, *, #7387, .T. ) ;
#218 = ORIENTED_EDGE ( 'NONE', *, *, #3634, .T. ) ;
#219 = CARTESIAN_POINT ( 'NONE',  ( 0.4685039370078740717, -0.1704774416898505729, -0.2952755905511810774 ) ) ;
#220 = LINE ( 'NONE', #7202, #7073 ) ;
#221 = CARTESIAN_POINT ( 'NONE',  ( -1.060348472569316414, 0.4341579012690653383, -1.570964862939435491 ) ) ;
#222 = CARTESIAN_POINT ( 'NONE',  ( 0.3485534891173983629, 0.1164145375797932258, -0.3017001449125945034 ) ) ;
#223 = VECTOR ( 'NONE', #79, 39.37007874015748143 ) ;
#224 = UNCERTAINTY_MEASURE_WITH_UNIT (LENGTH_MEASURE( 1.000000000000000082E-05 ), #1420, 'distance_accuracy_value', 'NONE');
#225 = CARTESIAN_POINT ( 'NONE',  ( 0.02637295201093697167, 0.1704774416898497680, -0.2952755905511810774 ) ) ;
#226 = FACE_BOUND ( 'NONE', #2302, .T. ) ;
#227 = CARTESIAN_POINT ( 'NONE',  ( -0.9609181420092316461, -0.5141614760841496379, -1.361499588670821659 ) ) ;
#228 = CARTESIAN_POINT ( 'NONE',  ( 0.3432736861146661878, -0.3267484299055466446, -0.02460629921259840577 ) ) ;
#229 = CARTESIAN_POINT ( 'NONE',  ( 0.3528971332113846615, 0.1886393090946605622, 0.2768874834731247514 ) ) ;
#230 = LINE ( 'NONE', #5471, #3282 ) ;
#231 = DIRECTION ( 'NONE',  ( -1.047444401652940007E-14, 1.000000000000000000, -0.000000000000000000 ) ) ;
#232 = ORIENTED_EDGE ( 'NONE', *, *, #1077, .T. ) ;
#233 = FACE_OUTER_BOUND ( 'NONE', #3715, .T. ) ;
#234 = ADVANCED_FACE ( 'NONE', ( #1554, #2883, #5130 ), #467, .T. ) ;
#235 = CARTESIAN_POINT ( 'NONE',  ( 0.3543307086614173596, -0.2045729300278204543, -0.3766201741223081378 ) ) ;
#236 = ORIENTED_EDGE ( 'NONE', *, *, #249, .T. ) ;
#237 = CIRCLE ( 'NONE', #7423, 1.223643328182682621 ) ;
#238 = ORIENTED_EDGE ( 'NONE', *, *, #6320, .T. ) ;
#239 = CARTESIAN_POINT ( 'NONE',  ( 0.3411144883932946681, 0.06120045565151401717, -0.3014953316451452481 ) ) ;
#240 = CARTESIAN_POINT ( 'NONE',  ( 0.1171503679538647841, -0.3415090635818134879, -0.003642820150508935782 ) ) ;
#241 = DIRECTION ( 'NONE',  ( 0.000000000000000000, 0.000000000000000000, 1.000000000000000000 ) ) ;
#242 = ORIENTED_EDGE ( 'NONE', *, *, #1147, .F. ) ;
#243 = CIRCLE ( 'NONE', #5500, 1.089828288828796676 ) ;
#244 = CARTESIAN_POINT ( 'NONE',  ( 0.4338950423154144254, -1.037563309807725043, -1.574803149606299302 ) ) ;
#245 = EDGE_CURVE ( 'NONE', #2222, #4734, #1124, .T. ) ;
#246 = EDGE_CURVE ( 'NONE', #5720, #477, #3388, .T. ) ;
#247 = ORIENTED_EDGE ( 'NONE', *, *, #6320, .F. ) ;
#248 = ORIENTED_EDGE ( 'NONE', *, *, #5809, .F. ) ;
#249 = EDGE_CURVE ( 'NONE', #6858, #951, #2962, .T. ) ;
#250 = FACE_OUTER_BOUND ( 'NONE', #326, .T. ) ;
#251 =( NAMED_UNIT ( * ) PLANE_ANGLE_UNIT ( ) SI_UNIT ( $, .RADIAN. ) );
#252 = CARTESIAN_POINT ( 'NONE',  ( 0.9666437042230172638, -0.4330708661417221883, -1.454455828411335583 ) ) ;
#253 = ORIENTED_EDGE ( 'NONE', *, *, #5052, .T. ) ;
#254 = CARTESIAN_POINT ( 'NONE',  ( 0.3561392902752972267, 0.3446605091515489439, -2.917830865379561131E-17 ) ) ;
#255 = ORIENTED_EDGE ( 'NONE', *, *, #2605, .T. ) ;
#256 = EDGE_CURVE ( 'NONE', #3323, #5932, #1903, .T. ) ;
#257 = AXIS2_PLACEMENT_3D ( 'NONE', #5618, #942, #371 ) ;
#258 = ORIENTED_EDGE ( 'NONE', *, *, #7198, .F. ) ;
#259 = CARTESIAN_POINT ( 'NONE',  ( 0.3543307086614173040, 0.2045729300278199825, -0.4082677165354330340 ) ) ;
#260 = CARTESIAN_POINT ( 'NONE',  ( 0.8791862816395774605, -0.2121393407445530399, -0.9611380397500175476 ) ) ;
#261 = DIRECTION ( 'NONE',  ( -0.000000000000000000, 0.000000000000000000, -1.000000000000000000 ) ) ;
#262 = CIRCLE ( 'NONE', #3188, 0.2362204724409449064 ) ;
#263 = CYLINDRICAL_SURFACE ( 'NONE', #3438, 0.2362204724409448231 ) ;
#264 = CARTESIAN_POINT ( 'NONE',  ( 0.3306743754077735575, 0.2557161625347751932, -0.1476377952755904832 ) ) ;
#265 = CARTESIAN_POINT ( 'NONE',  ( 0.3336175750056034062, -0.2273032555864673288, -0.1968503937007873295 ) ) ;
#266 = CARTESIAN_POINT ( 'NONE',  ( 0.3528850351813199171, 0.3340780101605773655, 0.02497973507596915402 ) ) ;
#267 = CARTESIAN_POINT ( 'NONE',  ( -0.4544645342395071674, 0.9861598787149296053, -1.560495034967182670 ) ) ;
#268 = DIRECTION ( 'NONE',  ( -1.000000000000000000, 0.000000000000000000, 0.000000000000000000 ) ) ;
#269 = VERTEX_POINT ( 'NONE', #2475 ) ;
#270 = PRODUCT_DEFINITION_SHAPE ( 'NONE', 'NONE',  #6029 ) ;
#271 = DIRECTION ( 'NONE',  ( -0.000000000000000000, -0.000000000000000000, 1.000000000000000000 ) ) ;
#272 = CARTESIAN_POINT ( 'NONE',  ( -0.4470331066954956190, 1.081428707249768362, -1.553789012478534959 ) ) ;
#273 = ORIENTED_EDGE ( 'NONE', *, *, #1681, .F. ) ;
#274 = AXIS2_PLACEMENT_3D ( 'NONE', #1457, #7244, #6147 ) ;
#275 = CARTESIAN_POINT ( 'NONE',  ( 0.01832242175888456129, 0.3270109559553079359, -0.02415159075610075201 ) ) ;
#276 = B_SPLINE_CURVE_WITH_KNOTS ( 'NONE', 3,
 ( #1085, #5765, #2842, #7501, #3460, #6940 ),
 .UNSPECIFIED., .F., .F.,
 ( 4, 2, 4 ),
 ( -3.269571951034336179E-06, 0.0001651384380483830793, 0.0003335464480478004612 ),
 .UNSPECIFIED. ) ;
#277 = CARTESIAN_POINT ( 'NONE',  ( -0.4330708661417317362, -1.044891351410288438, -1.574550377471545914 ) ) ;
#278 = VECTOR ( 'NONE', #577, 39.37007874015748143 ) ;
#279 = CARTESIAN_POINT ( 'NONE',  ( 1.055789886223273654E-16, -0.2411939993270979798, -0.1727909197870958757 ) ) ;
#280 = ORIENTED_EDGE ( 'NONE', *, *, #4164, .F. ) ;
#281 = AXIS2_PLACEMENT_3D ( 'NONE', #6819, #5069, #5106 ) ;
#282 = LINE ( 'NONE', #5487, #1734 ) ;
#283 = VERTEX_POINT ( 'NONE', #1196 ) ;
#284 = VECTOR ( 'NONE', #6774, 39.37007874015748143 ) ;
#285 = LINE ( 'NONE', #398, #6742 ) ;
#286 = APPLICATION_CONTEXT ( 'automotive_design' ) ;
#287 = EDGE_CURVE ( 'NONE', #5534, #7462, #1651, .T. ) ;
#288 = CARTESIAN_POINT ( 'NONE',  ( 0.000000000000000000, 0.000000000000000000, 0.000000000000000000 ) ) ;
#289 = ORIENTED_EDGE ( 'NONE', *, *, #5761, .F. ) ;
#290 = CARTESIAN_POINT ( 'NONE',  ( -0.1771653543307088186, -0.3068593950417299876, 7.886165872636028972E-17 ) ) ;
#291 = ORIENTED_EDGE ( 'NONE', *, *, #6914, .T. ) ;
#292 = LINE ( 'NONE', #4459, #6747 ) ;
#293 = ORIENTED_EDGE ( 'NONE', *, *, #4904, .T. ) ;
#294 = CIRCLE ( 'NONE', #4189, 0.2362204724409448231 ) ;
#295 = CARTESIAN_POINT ( 'NONE',  ( 0.000000000000000000, 0.000000000000000000, 0.000000000000000000 ) ) ;
#296 =( GEOMETRIC_REPRESENTATION_CONTEXT ( 3 ) GLOBAL_UNCERTAINTY_ASSIGNED_CONTEXT ( ( #7477 ) ) GLOBAL_UNIT_ASSIGNED_CONTEXT ( ( #4575, #4535, #6833 ) ) REPRESENTATION_CONTEXT ( 'NONE', 'WORKASPACE' ) );
#297 = EDGE_LOOP ( 'NONE', ( #6707, #7218, #922, #3341 ) ) ;
#298 = EDGE_CURVE ( 'NONE', #1329, #4949, #6196, .T. ) ;
#299 = ADVANCED_FACE ( 'NONE', ( #2390, #602, #105 ), #1773, .T. ) ;
#300 = PLANE ( 'NONE',  #6109 ) ;
#301 = AXIS2_PLACEMENT_3D ( 'NONE', #5704, #2813, #2276 ) ;
#302 = UNCERTAINTY_MEASURE_WITH_UNIT (LENGTH_MEASURE( 1.000000000000000082E-05 ), #3871, 'distance_accuracy_value', 'NONE');
#303 = SHAPE_REPRESENTATION ( 'MAT-019', ( #2876, #6981, #3696, #400, #2937, #394, #7219, #2826, #3559, #7102, #527, #5772, #2463, #4657, #4651, #1352, #2328, #6621, #20, #4231, #78, #1286, #5820, #6308, #331, #5714, #6188, #5094, #2520, #2389, #1155, #2036, #7031, #1772, #4712 ), #4840 ) ;
#304 = CARTESIAN_POINT ( 'NONE',  ( 0.4837908950006664655, -1.080458485393811729, -1.514208454829284234 ) ) ;
#305 = CLOSED_SHELL ( 'NONE', ( #1149, #6868, #3499, #5163, #6222, #1636, #5575, #2053, #3601, #534, #3181, #4486, #5802, #2374, #6509, #6038, #2797, #4111, #3420, #2152, #3035, #947, #2811, #6077, #4630, #5716, #6046, #5573, #7144, #802, #7479, #5229, #6436 ) ) ;
#306 = CYLINDRICAL_SURFACE ( 'NONE', #3807, 0.2362204724409455170 ) ;
#307 = DIRECTION ( 'NONE',  ( -0.000000000000000000, -0.000000000000000000, -1.000000000000000000 ) ) ;
#308 = DIRECTION ( 'NONE',  ( -2.312579046053608732E-29, 2.207829878515936732E-15, 1.000000000000000000 ) ) ;
#309 = CARTESIAN_POINT ( 'NONE',  ( -0.4509662133831515707, 0.9917530546321599028, -1.563429817131423372 ) ) ;
#310 = B_SPLINE_CURVE_WITH_KNOTS ( 'NONE', 3,
 ( #2397, #7457, #2193, #4023, #4600, #2234, #4565, #4489 ),
 .UNSPECIFIED., .F., .F.,
 ( 4, 2, 2, 4 ),
 ( 0.004381617662950710798, 0.005472867551409541474, 0.006564117439868372150, 0.008746617216786031768 ),
 .UNSPECIFIED. ) ;
#311 = EDGE_LOOP ( 'NONE', ( #1043, #2728, #1834, #6345 ) ) ;
#312 = CARTESIAN_POINT ( 'NONE',  ( 0.02637295201093751290, -0.3409548833797009237, -9.138209691400258722E-18 ) ) ;
#313 = DIRECTION ( 'NONE',  ( -0.000000000000000000, -0.000000000000000000, 1.000000000000000000 ) ) ;
#314 = ADVANCED_BREP_SHAPE_REPRESENTATION ( '', ( #1545, #5166 ), #1473 ) ;
#315 = ORIENTED_EDGE ( 'NONE', *, *, #97, .T. ) ;
#316 = CARTESIAN_POINT ( 'NONE',  ( 0.9055118110236223261, 0.7480314960629921295, -0.7480314960629921295 ) ) ;
#317 = CARTESIAN_POINT ( 'NONE',  ( 0.3322355029819564209, 0.06185644463604170890, -0.2952755905511810774 ) ) ;
#318 = DIRECTION ( 'NONE',  ( 0.000000000000000000, -4.647695938698650194E-15, 1.000000000000000000 ) ) ;
#319 = ORIENTED_EDGE ( 'NONE', *, *, #4766, .T. ) ;
#320 = CARTESIAN_POINT ( 'NONE',  ( 0.4700904924197906176, -0.9659644734970541657, -1.546597720061111847 ) ) ;
#321 = VERTEX_POINT ( 'NONE', #3584 ) ;
#322 = VERTEX_POINT ( 'NONE', #3083 ) ;
#323 = CARTESIAN_POINT ( 'NONE',  ( -0.4330708661417322913, 0.9666437042230143772, -1.454455828411337359 ) ) ;
#324 = CARTESIAN_POINT ( 'NONE',  ( 0.4330708661417322913, -1.048552902599920289, -1.573978973432616835 ) ) ;
#325 = CARTESIAN_POINT ( 'NONE',  ( 0.9984400756355499285, -0.4637694296357074975, -1.410742812766314414 ) ) ;
#326 = EDGE_LOOP ( 'NONE', ( #3963, #5644, #3881, #5352 ) ) ;
#327 = CARTESIAN_POINT ( 'NONE',  ( 0.9454567723360981502, 0.2331403729576253803, 0.9562426076827387211 ) ) ;
#328 = ORIENTED_EDGE ( 'NONE', *, *, #2423, .F. ) ;
#329 = EDGE_CURVE ( 'NONE', #1607, #4990, #5298, .T. ) ;
#330 = ORIENTED_EDGE ( 'NONE', *, *, #1146, .F. ) ;
#331 = AXIS2_PLACEMENT_3D ( 'NONE', #1757, #3459, #3489 ) ;
#332 = ORIENTED_EDGE ( 'NONE', *, *, #2879, .T. ) ;
#333 = DIRECTION ( 'NONE',  ( -0.8340899802305957733, 0.5516284119576553291, -1.062608521779998955E-15 ) ) ;
#334 = PRODUCT_DEFINITION_SHAPE ( 'NONE', 'NONE',  #1953 ) ;
#335 = FACE_OUTER_BOUND ( 'NONE', #5189, .T. ) ;
#336 = DIRECTION ( 'NONE',  ( -0.8660254037844382635, 0.5000000000000006661, 0.000000000000000000 ) ) ;
#337 = DIRECTION ( 'NONE',  ( -1.000000000000000000, -8.881784197001252323E-16, 0.000000000000000000 ) ) ;
#338 = CARTESIAN_POINT ( 'NONE',  ( 0.8465112843344620996, 0.1920587529112295633, -0.9653415754825105388 ) ) ;
#339 = EDGE_CURVE ( 'NONE', #5905, #4449, #1926, .T. ) ;
#340 = EDGE_CURVE ( 'NONE', #1419, #4225, #5767, .T. ) ;
#341 = CARTESIAN_POINT ( 'NONE',  ( 0.4330708661417322913, 1.048552902599920289, -1.573978973432616835 ) ) ;
#342 = DIRECTION ( 'NONE',  ( -1.000000000000000000, 0.000000000000000000, -0.000000000000000000 ) ) ;
#343 = FACE_OUTER_BOUND ( 'NONE', #5945, .T. ) ;
#344 = CARTESIAN_POINT ( 'NONE',  ( -2.834645669291338432, 0.000000000000000000, 2.952755905511811108 ) ) ;
#345 = VERTEX_POINT ( 'NONE', #7020 ) ;
#346 = MECHANICAL_DESIGN_GEOMETRIC_PRESENTATION_REPRESENTATION (  '', ( #1785 ), #5726 ) ;
#347 = CARTESIAN_POINT ( 'NONE',  ( -0.9971723906835432416, 0.4475999628372159256, -1.429777239771657049 ) ) ;
#348 = ORIENTED_EDGE ( 'NONE', *, *, #6732, .T. ) ;
#349 = CARTESIAN_POINT ( 'NONE',  ( -0.1771653543307089573, 0.3068593950417301541, -0.4082677165354330340 ) ) ;
#350 = PLANE ( 'NONE',  #1220 ) ;
#351 = CONICAL_SURFACE ( 'NONE', #1424, 0.2952755905511810774, 1.047197551196600518 ) ;
#352 = CONTEXT_DEPENDENT_SHAPE_REPRESENTATION ( #1183, #5460 ) ;
#353 = CARTESIAN_POINT ( 'NONE',  ( 0.3432736861146661322, -0.1846838951640047688, -0.2706692913385826404 ) ) ;
#354 = ORIENTED_EDGE ( 'NONE', *, *, #7147, .F. ) ;
#355 = CARTESIAN_POINT ( 'NONE',  ( 0.4617902729098475878, -0.9752011746066220343, -1.554226146211406423 ) ) ;
#356 = AXIS2_PLACEMENT_3D ( 'NONE', #2044, #3186, #894 ) ;
#357 = EDGE_LOOP ( 'NONE', ( #3994, #2629, #763 ) ) ;
#358 = VERTEX_POINT ( 'NONE', #7135 ) ;
#359 = DIRECTION ( 'NONE',  ( 0.000000000000000000, 0.000000000000000000, -1.000000000000000000 ) ) ;
#360 = FACE_OUTER_BOUND ( 'NONE', #1560, .T. ) ;
#361 = AXIS2_PLACEMENT_3D ( 'NONE', #4889, #1987, #872 ) ;
#362 = SURFACE_STYLE_FILL_AREA ( #4370 ) ;
#363 = ORIENTED_EDGE ( 'NONE', *, *, #1119, .T. ) ;
#364 = EDGE_LOOP ( 'NONE', ( #2793, #2733, #2565, #4438 ) ) ;
#365 = CARTESIAN_POINT ( 'NONE',  ( -1.795185198899834826E-15, 0.5141614760841457521, -2.204724409448820754 ) ) ;
#366 = CARTESIAN_POINT ( 'NONE',  ( 0.3337354549120238878, 0.2853048623713461129, 0.09638866382874489158 ) ) ;
#367 = EDGE_LOOP ( 'NONE', ( #1959, #4482 ) ) ;
#368 = CIRCLE ( 'NONE', #6106, 0.03543307086614165546 ) ;
#369 = CARTESIAN_POINT ( 'NONE',  ( -0.9842519685039370358, 1.220472440944881942, 0.000000000000000000 ) ) ;
#370 = DIRECTION ( 'NONE',  ( 0.9991895563372417133, -0.04025208698423568543, 8.278313773160990025E-16 ) ) ;
#371 = DIRECTION ( 'NONE',  ( 0.000000000000000000, 0.000000000000000000, 1.000000000000000000 ) ) ;
#372 = CARTESIAN_POINT ( 'NONE',  ( 21.65354330708661479, 0.000000000000000000, 0.4921259842519685179 ) ) ;
#373 = VECTOR ( 'NONE', #3196, 39.37007874015748143 ) ;
#374 = CARTESIAN_POINT ( 'NONE',  ( 0.05817553349160906745, 0.3755582001340100340, -0.3942397458900142593 ) ) ;
#375 = CARTESIAN_POINT ( 'NONE',  ( 0.7601524118086268045, 0.07627561187719542057, -0.9813965260305658189 ) ) ;
#376 = EDGE_CURVE ( 'NONE', #1383, #931, #426, .T. ) ;
#377 = ADVANCED_FACE ( 'NONE', ( #186 ), #5685, .F. ) ;
#378 = DIRECTION ( 'NONE',  ( 1.000000000000000000, 0.000000000000000000, 0.000000000000000000 ) ) ;
#379 = CYLINDRICAL_SURFACE ( 'NONE', #5488, 1.968503937007874072 ) ;
#380 = AXIS2_PLACEMENT_3D ( 'NONE', #4053, #3479, #6788 ) ;
#381 = CARTESIAN_POINT ( 'NONE',  ( -1.279527559055117836, 1.968503937007873850, 2.952755905511811108 ) ) ;
#382 = EDGE_CURVE ( 'NONE', #2732, #3031, #1272, .T. ) ;
#383 = VERTEX_POINT ( 'NONE', #4689 ) ;
#384 = CARTESIAN_POINT ( 'NONE',  ( 0.002513486811083454845, 0.2268523693227592619, 0.1976313516179636909 ) ) ;
#385 = CARTESIAN_POINT ( 'NONE',  ( 0.3485777078273626373, -0.2029921329169081246, -0.2518088348849962799 ) ) ;
#386 = AXIS2_PLACEMENT_3D ( 'NONE', #757, #3705, #6044 ) ;
#387 = EDGE_CURVE ( 'NONE', #3423, #6545, #3883, .T. ) ;
#388 = ITEM_DEFINED_TRANSFORMATION ( 'NONE', 'NONE', #2826,  #5166 ) ;
#389 = EDGE_CURVE ( 'NONE', #6862, #321, #1535, .T. ) ;
#390 = CARTESIAN_POINT ( 'NONE',  ( -0.9895441027518975252, -0.4843356560173227576, -1.389133886014303654 ) ) ;
#391 = ORIENTED_EDGE ( 'NONE', *, *, #2568, .F. ) ;
#392 = CARTESIAN_POINT ( 'NONE',  ( 0.000000000000000000, 0.000000000000000000, 0.1188976377952756375 ) ) ;
#393 = CARTESIAN_POINT ( 'NONE',  ( 0.3459463601587710602, -0.3157502742997210787, 0.04365566351110977683 ) ) ;
#394 = AXIS2_PLACEMENT_3D ( 'NONE', #452, #3847, #6749 ) ;
#395 = ORIENTED_EDGE ( 'NONE', *, *, #1081, .F. ) ;
#396 = TOROIDAL_SURFACE ( 'NONE', #4047, 0.4507874015748032370, 0.03543307086614166934 ) ;
#397 = ORIENTED_EDGE ( 'NONE', *, *, #2431, .F. ) ;
#398 = CARTESIAN_POINT ( 'NONE',  ( 0.000000000000000000, 1.496062992125984259, 0.7480314960629921295 ) ) ;
#399 = MECHANICAL_DESIGN_GEOMETRIC_PRESENTATION_REPRESENTATION (  '', ( #7343 ), #5389 ) ;
#400 = AXIS2_PLACEMENT_3D ( 'NONE', #2650, #1049, #494 ) ;
#401 = CARTESIAN_POINT ( 'NONE',  ( 0.3432736861146661878, -0.1420645347415422088, -0.2952755905511810774 ) ) ;
#402 = ORIENTED_EDGE ( 'NONE', *, *, #6794, .T. ) ;
#403 = CARTESIAN_POINT ( 'NONE',  ( 0.4338950423154144254, 1.037563309807724821, -1.574803149606299302 ) ) ;
#404 = ORIENTED_EDGE ( 'NONE', *, *, #5065, .F. ) ;
#405 = CARTESIAN_POINT ( 'NONE',  ( -0.3543307086614173040, 0.000000000000000000, -0.4082677165354330340 ) ) ;
#406 = ORIENTED_EDGE ( 'NONE', *, *, #5878, .F. ) ;
#407 = CARTESIAN_POINT ( 'NONE',  ( 0.3411151615605803600, 0.2304996462388439749, 0.2037536041052391000 ) ) ;
#408 = VERTEX_POINT ( 'NONE', #1981 ) ;
#409 = CIRCLE ( 'NONE', #3943, 1.278433327952055887 ) ;
#410 = DIRECTION ( 'NONE',  ( -0.000000000000000000, -0.000000000000000000, 1.000000000000000000 ) ) ;
#411 = DIRECTION ( 'NONE',  ( 5.157119279398578587E-32, 1.000000000000000222, -1.795077641733700520E-27 ) ) ;
#412 = DIRECTION ( 'NONE',  ( -1.000000000000000000, -0.000000000000000000, -0.000000000000000000 ) ) ;
#413 = DIRECTION ( 'NONE',  ( 1.000000000000000000, 0.000000000000000000, -0.000000000000000000 ) ) ;
#414 = CARTESIAN_POINT ( 'NONE',  ( 0.9530933633567026941, -0.2342849080887553226, -0.9559618965236083010 ) ) ;
#415 = AXIS2_PLACEMENT_3D ( 'NONE', #4819, #7026, #1709 ) ;
#416 = DIRECTION ( 'NONE',  ( 0.000000000000000000, -4.615976749461841764E-15, 1.000000000000000000 ) ) ;
#417 = CARTESIAN_POINT ( 'NONE',  ( 1.140380516255546706, 0.1779313096650642356, -0.9680979248264950376 ) ) ;
#418 = CARTESIAN_POINT ( 'NONE',  ( 0.000000000000000000, 0.000000000000000000, 0.000000000000000000 ) ) ;
#419 = CARTESIAN_POINT ( 'NONE',  ( 0.000000000000000000, 0.000000000000000000, -1.546597720061111847 ) ) ;
#420 = CARTESIAN_POINT ( 'NONE',  ( 2.892866454678787531E-17, 1.496062992125984259, 0.2362204724409449341 ) ) ;
#421 = CARTESIAN_POINT ( 'NONE',  ( 0.3479980290963757827, -0.3208941761713900997, 0.04760384692073289098 ) ) ;
#422 = CARTESIAN_POINT ( 'NONE',  ( 1.023372273685344114, -0.4368378848980421503, -1.573834172653142627 ) ) ;
#423 = DIRECTION ( 'NONE',  ( 0.000000000000000000, 0.000000000000000000, 1.000000000000000000 ) ) ;
#424 = ORIENTED_EDGE ( 'NONE', *, *, #923, .T. ) ;
#425 = CARTESIAN_POINT ( 'NONE',  ( -0.4338950423154138147, 1.037563309807725043, -1.574803149606299302 ) ) ;
#426 = CIRCLE ( 'NONE', #548, 0.2952755905511810774 ) ;
#427 = EDGE_CURVE ( 'NONE', #4734, #3441, #198, .T. ) ;
#428 = VERTEX_POINT ( 'NONE', #369 ) ;
#429 = DIRECTION ( 'NONE',  ( -1.000000000000000000, -0.000000000000000000, -0.000000000000000000 ) ) ;
#430 = CARTESIAN_POINT ( 'NONE',  ( 0.000000000000000000, 0.2066929133858267931, 0.1188976377952756375 ) ) ;
#431 = CONTEXT_DEPENDENT_SHAPE_REPRESENTATION ( #6780, #1976 ) ;
#432 = VECTOR ( 'NONE', #5331, 39.37007874015748143 ) ;
#433 = CARTESIAN_POINT ( 'NONE',  ( 0.3543307086614173040, 0.2045729300278205931, -0.03164754241312491001 ) ) ;
#434 = EDGE_LOOP ( 'NONE', ( #1915, #6428, #3869, #6323 ) ) ;
#436 = DIMENSIONAL_EXPONENTS ( 1.000000000000000000, 0.000000000000000000, 0.000000000000000000, 0.000000000000000000, 0.000000000000000000, 0.000000000000000000, 0.000000000000000000 ) ;
#435 = CARTESIAN_POINT ( 'NONE',  ( 0.3487102105009307618, 0.2024297391849447236, -0.2527898980517343519 ) ) ;
#437 = CARTESIAN_POINT ( 'NONE',  ( 0.3411151615605706455, -0.2917056203871725706, 0.09774174715353350917 ) ) ;
#438 = APPLICATION_CONTEXT ( 'automotive_design' ) ;
#439 = AXIS2_PLACEMENT_3D ( 'NONE', #7431, #5193, #1051 ) ;
#440 = ADVANCED_FACE ( 'NONE', ( #4884 ), #5559, .T. ) ;
#441 = ADVANCED_FACE ( 'NONE', ( #1579 ), #4944, .F. ) ;
#442 = ORIENTED_EDGE ( 'NONE', *, *, #702, .F. ) ;
#443 = VERTEX_POINT ( 'NONE', #5112 ) ;
#444 = DIRECTION ( 'NONE',  ( 1.000000000000000000, 0.000000000000000000, 0.000000000000000000 ) ) ;
#445 = CARTESIAN_POINT ( 'NONE',  ( 0.3306743754077733910, -4.012401740694386787E-16, -0.2952755905511810774 ) ) ;
#446 = ORIENTED_EDGE ( 'NONE', *, *, #5897, .F. ) ;
#447 = LINE ( 'NONE', #1687, #103 ) ;
#448 = VERTEX_POINT ( 'NONE', #6828 ) ;
#449 = CARTESIAN_POINT ( 'NONE',  ( -0.2520187439128739326, -0.2636427704167116359, -0.4024809188492813328 ) ) ;
#450 = VERTEX_POINT ( 'NONE', #1357 ) ;
#451 = CARTESIAN_POINT ( 'NONE',  ( 0.000000000000000000, 0.000000000000000000, -0.7983802283864783744 ) ) ;
#452 = CARTESIAN_POINT ( 'NONE',  ( 18.41860179314716461, 41.48855051017370243, 54.13003647711799715 ) ) ;
#453 = CARTESIAN_POINT ( 'NONE',  ( 0.000000000000000000, 0.2559055118110236116, 0.000000000000000000 ) ) ;
#454 = CARTESIAN_POINT ( 'NONE',  ( 0.7480314960629922405, 1.220472440944881942, 0.4724409448818898127 ) ) ;
#455 =( LENGTH_UNIT ( ) NAMED_UNIT ( * ) SI_UNIT ( $, .METRE. ) );
#456 = CARTESIAN_POINT ( 'NONE',  ( 0.02637295201093722841, 0.3409548833797004797, 3.882420715168025960E-18 ) ) ;
#457 = B_SPLINE_CURVE_WITH_KNOTS ( 'NONE', 3,
 ( #7261, #6093, #2034, #3246, #847, #5522, #7295, #3212, #1442, #883, #1478, #3832, #6164, #4825, #7148, #4247, #6583, #1332 ),
 .UNSPECIFIED., .F., .F.,
 ( 4, 2, 2, 2, 2, 2, 2, 2, 4 ),
 ( -8.042425861382277794E-06, 0.0009212656149224035746, 0.001385919635314291623, 0.001850573655706179562, 0.002315227676098066852, 0.002779881696489955225, 0.003244535716881843165, 0.003476862727077782798, 0.003709189737273722864 ),
 .UNSPECIFIED. ) ;
#458 =( LENGTH_UNIT ( ) NAMED_UNIT ( * ) SI_UNIT ( $, .METRE. ) );
#459 = EDGE_CURVE ( 'NONE', #2045, #4474, #3812, .T. ) ;
#460 = LINE ( 'NONE', #561, #3345 ) ;
#461 = CARTESIAN_POINT ( 'NONE',  ( 0.3426144402834003788, -0.2318662757222078041, 0.2014770286013906619 ) ) ;
#462 = LINE ( 'NONE', #2137, #1177 ) ;
#463 = EDGE_LOOP ( 'NONE', ( #2691, #1742, #5296, #4406 ) ) ;
#464 = UNCERTAINTY_MEASURE_WITH_UNIT (LENGTH_MEASURE( 1.000000000000000082E-05 ), #7315, 'distance_accuracy_value', 'NONE');
#465 = DIRECTION ( 'NONE',  ( 0.000000000000000000, 1.000000000000000000, 0.000000000000000000 ) ) ;
#466 = ORIENTED_EDGE ( 'NONE', *, *, #3634, .F. ) ;
#467 = PLANE ( 'NONE',  #1133 ) ;
#468 = CARTESIAN_POINT ( 'NONE',  ( 0.3426147637089221321, -0.05832033309504448121, 0.3015404986019939448 ) ) ;
#469 = DIRECTION ( 'NONE',  ( 0.000000000000000000, -0.000000000000000000, 1.000000000000000000 ) ) ;
#470 = VECTOR ( 'NONE', #3256, 39.37007874015748143 ) ;
#471 = CARTESIAN_POINT ( 'NONE',  ( -0.9697097640641200167, -0.4330708661417358440, -1.453662949853145481 ) ) ;
#472 = ORIENTED_EDGE ( 'NONE', *, *, #7389, .F. ) ;
#473 = CARTESIAN_POINT ( 'NONE',  ( 0.01168997831664882192, -0.1984671517595423818, -0.2467959906213527677 ) ) ;
#474 = DIRECTION ( 'NONE',  ( -1.000000000000000000, -0.000000000000000000, -0.000000000000000000 ) ) ;
#475 = ORIENTED_EDGE ( 'NONE', *, *, #2364, .T. ) ;
#476 = AXIS2_PLACEMENT_3D ( 'NONE', #6453, #2355, #607 ) ;
#477 = VERTEX_POINT ( 'NONE', #6294 ) ;
#478 = B_SPLINE_CURVE_WITH_KNOTS ( 'NONE', 3,
 ( #3784, #4893, #6118, #2631, #4971, #1948 ),
 .UNSPECIFIED., .F., .F.,
 ( 4, 2, 4 ),
 ( 0.000000000000000000, 0.0001677595217559108194, 0.0003355190435118216388 ),
 .UNSPECIFIED. ) ;
#479 = DIRECTION ( 'NONE',  ( 0.000000000000000000, 0.000000000000000000, -1.000000000000000000 ) ) ;
#480 = PLANE ( 'NONE',  #3038 ) ;
#481 = EDGE_CURVE ( 'NONE', #2228, #951, #4333, .T. ) ;
#482 = CARTESIAN_POINT ( 'NONE',  ( 0.02637295201093751290, -0.3409548833797009237, -9.138209691400258722E-18 ) ) ;
#483 = ORIENTED_EDGE ( 'NONE', *, *, #6552, .F. ) ;
#484 = EDGE_CURVE ( 'NONE', #2382, #4304, #1169, .T. ) ;
#485 = CARTESIAN_POINT ( 'NONE',  ( 0.3483227611829849413, -0.3409548833797009237, 0.000000000000000000 ) ) ;
#486 = EDGE_LOOP ( 'NONE', ( #5349, #1848, #4162 ) ) ;
#487 = CARTESIAN_POINT ( 'NONE',  ( -0.8785537298370134085, 0.4700904924197875645, -1.433776001880362250 ) ) ;
#488 = EDGE_CURVE ( 'NONE', #4739, #1108, #3971, .T. ) ;
#489 = VERTEX_POINT ( 'NONE', #3117 ) ;
#490 = DIMENSIONAL_EXPONENTS ( 1.000000000000000000, 0.000000000000000000, 0.000000000000000000, 0.000000000000000000, 0.000000000000000000, 0.000000000000000000, 0.000000000000000000 ) ;
#491 = EDGE_LOOP ( 'NONE', ( #3148, #2683 ) ) ;
#492 = PLANE ( 'NONE',  #7107 ) ;
#493 = VECTOR ( 'NONE', #4622, 39.37007874015748143 ) ;
#494 = DIRECTION ( 'NONE',  ( 0.9930405933431722953, -2.114621326752049776E-28, -0.1177725773371735979 ) ) ;
#495 = CARTESIAN_POINT ( 'NONE',  ( 0.000000000000000000, 0.000000000000000000, -0.8561751947315059397 ) ) ;
#496 = EDGE_CURVE ( 'NONE', #951, #5211, #3383, .T. ) ;
#497 = CARTESIAN_POINT ( 'NONE',  ( -0.1470270249832137943, 0.3242597676034320586, -0.4075196867561205472 ) ) ;
#498 = B_SPLINE_CURVE_WITH_KNOTS ( 'NONE', 3,
 ( #801, #3127, #3279, #3396, #6338, #6232, #6305, #2138 ),
 .UNSPECIFIED., .F., .F.,
 ( 4, 2, 2, 4 ),
 ( 0.005257893453559879353, 0.006567392922673220834, 0.007876892391786561448, 0.01049589133001324961 ),
 .UNSPECIFIED. ) ;
#499 = CIRCLE ( 'NONE', #5364, 0.4629062255509093782 ) ;
#500 = CARTESIAN_POINT ( 'NONE',  ( -0.3543307086614173040, 0.000000000000000000, -0.4082677165354330340 ) ) ;
#501 = AXIS2_PLACEMENT_3D ( 'NONE', #5115, #2243, #3385 ) ;
#502 = CARTESIAN_POINT ( 'NONE',  ( 0.3485373078438445127, -0.3194486952732369378, -0.05009812457233156491 ) ) ;
#503 = FACE_OUTER_BOUND ( 'NONE', #3481, .T. ) ;
#504 = FACE_OUTER_BOUND ( 'NONE', #119, .T. ) ;
#505 = LINE ( 'NONE', #2311, #5123 ) ;
#506 = LINE ( 'NONE', #4473, #4310 ) ;
#507 =( GEOMETRIC_REPRESENTATION_CONTEXT ( 3 ) GLOBAL_UNCERTAINTY_ASSIGNED_CONTEXT ( ( #4584 ) ) GLOBAL_UNIT_ASSIGNED_CONTEXT ( ( #6521, #15, #6473 ) ) REPRESENTATION_CONTEXT ( 'NONE', 'WORKASPACE' ) );
#508 = FACE_OUTER_BOUND ( 'NONE', #2139, .T. ) ;
#509 = CARTESIAN_POINT ( 'NONE',  ( 0.3425764178929370796, -0.2900721174007588332, -0.1006592143205869427 ) ) ;
#510 = CARTESIAN_POINT ( 'NONE',  ( -0.9666437042230129340, -0.4330708661417356220, -1.454455828411337359 ) ) ;
#511 = ORIENTED_EDGE ( 'NONE', *, *, #6690, .T. ) ;
#512 = DIRECTION ( 'NONE',  ( 0.000000000000000000, 0.000000000000000000, -1.000000000000000000 ) ) ;
#513 = DIRECTION ( 'NONE',  ( -1.000000000000000000, -0.000000000000000000, -0.000000000000000000 ) ) ;
#514 = ORIENTED_EDGE ( 'NONE', *, *, #5753, .T. ) ;
#515 = CIRCLE ( 'NONE', #3926, 1.174991162294038993 ) ;
#516 = ORIENTED_EDGE ( 'NONE', *, *, #4216, .T. ) ;
#517 = CARTESIAN_POINT ( 'NONE',  ( 0.8226608724162054465, -0.1724771829768798059, 0.9690378908208601150 ) ) ;
#518 = DIRECTION ( 'NONE',  ( 0.000000000000000000, 0.000000000000000000, 1.000000000000000000 ) ) ;
#519 = ORIENTED_EDGE ( 'NONE', *, *, #1924, .T. ) ;
#520 = LINE ( 'NONE', #3297, #3400 ) ;
#521 = ORIENTED_EDGE ( 'NONE', *, *, #1115, .F. ) ;
#522 = VECTOR ( 'NONE', #4279, 39.37007874015748143 ) ;
#523 = DIRECTION ( 'NONE',  ( 1.000000000000000000, 0.000000000000000000, 0.000000000000000000 ) ) ;
#524 = ORIENTED_EDGE ( 'NONE', *, *, #6050, .T. ) ;
#525 = ADVANCED_FACE ( 'NONE', ( #5728 ), #53, .T. ) ;
#526 = VECTOR ( 'NONE', #2960, 39.37007874015748143 ) ;
#527 = AXIS2_PLACEMENT_3D ( 'NONE', #2693, #370, #2129 ) ;
#528 = CARTESIAN_POINT ( 'NONE',  ( 0.3543307086614172485, 0.000000000000000000, 7.886165872636028972E-17 ) ) ;
#529 = DIRECTION ( 'NONE',  ( 0.000000000000000000, 0.000000000000000000, -1.000000000000000000 ) ) ;
#530 = AXIS2_PLACEMENT_3D ( 'NONE', #2041, #6853, #2680 ) ;
#531 = FACE_OUTER_BOUND ( 'NONE', #736, .T. ) ;
#532 = DIRECTION ( 'NONE',  ( 0.000000000000000000, 0.000000000000000000, 1.000000000000000000 ) ) ;
#533 = ADVANCED_FACE ( 'NONE', ( #4495 ), #6902, .F. ) ;
#534 = ADVANCED_FACE ( 'NONE', ( #2338 ), #7464, .F. ) ;
#535 = AXIS2_PLACEMENT_3D ( 'NONE', #6664, #2000, #1481 ) ;
#536 =( REPRESENTATION_RELATIONSHIP ('NONE','NONE', #303, #5265 ) REPRESENTATION_RELATIONSHIP_WITH_TRANSFORMATION ( #109 )SHAPE_REPRESENTATION_RELATIONSHIP( ) );
#537 = CARTESIAN_POINT ( 'NONE',  ( 0.3528850351813199726, -0.3340780101605776986, -0.02497973507596915055 ) ) ;
#538 = PLANE ( 'NONE',  #6985 ) ;
#539 = DIRECTION ( 'NONE',  ( 0.000000000000000000, 0.000000000000000000, 1.000000000000000000 ) ) ;
#540 = CARTESIAN_POINT ( 'NONE',  ( 0.000000000000000000, 1.496062992125984259, -0.4921259842519685179 ) ) ;
#541 = CARTESIAN_POINT ( 'NONE',  ( 0.3543307086614173040, 0.2045729300278205931, -0.3766201741223081378 ) ) ;
#542 = DIRECTION ( 'NONE',  ( 0.000000000000000000, -0.5000000000000005551, 0.8660254037844382635 ) ) ;
#543 = ORIENTED_EDGE ( 'NONE', *, *, #1482, .T. ) ;
#544 = DIRECTION ( 'NONE',  ( 0.000000000000000000, 1.000000000000000000, 0.000000000000000000 ) ) ;
#545 = CARTESIAN_POINT ( 'NONE',  ( -2.834645669291338432, 0.4724409448818898127, 0.000000000000000000 ) ) ;
#546 = ORIENTED_EDGE ( 'NONE', *, *, #1729, .T. ) ;
#547 = ORIENTED_EDGE ( 'NONE', *, *, #3754, .F. ) ;
#548 = AXIS2_PLACEMENT_3D ( 'NONE', #5429, #4233, #3005 ) ;
#549 = CARTESIAN_POINT ( 'NONE',  ( 1.196439825128248202, -0.1049569639594290504, 0.9787451009560118598 ) ) ;
#550 = ORIENTED_EDGE ( 'NONE', *, *, #3088, .T. ) ;
#551 = CARTESIAN_POINT ( 'NONE',  ( 0.4700904924197903956, 0.000000000000000000, -2.204724409448820754 ) ) ;
#552 = DIRECTION ( 'NONE',  ( -1.000000000000000000, 0.000000000000000000, 0.000000000000000000 ) ) ;
#553 = ORIENTED_EDGE ( 'NONE', *, *, #3600, .F. ) ;
#554 = ORIENTED_EDGE ( 'NONE', *, *, #5878, .T. ) ;
#555 = DIRECTION ( 'NONE',  ( 0.000000000000000000, 0.000000000000000000, 1.000000000000000000 ) ) ;
#556 = LINE ( 'NONE', #177, #2443 ) ;
#557 = CARTESIAN_POINT ( 'NONE',  ( -0.9604263920613177463, -0.4330708661417355665, -1.456063616177416087 ) ) ;
#558 = PRODUCT_DEFINITION ( 'UNKNOWN', '', #6558, #2961 ) ;
#559 = SURFACE_STYLE_FILL_AREA ( #6369 ) ;
#560 = CARTESIAN_POINT ( 'NONE',  ( 0.4685039370078740717, 0.000000000000000000, 0.000000000000000000 ) ) ;
#561 = CARTESIAN_POINT ( 'NONE',  ( 0.000000000000000000, 0.000000000000000000, 0.2362204724409449064 ) ) ;
#562 = EDGE_CURVE ( 'NONE', #4139, #6455, #5693, .T. ) ;
#563 = CARTESIAN_POINT ( 'NONE',  ( 0.5118110236220474452, 1.220472440944881942, 0.000000000000000000 ) ) ;
#564 = CARTESIAN_POINT ( 'NONE',  ( -5.154746071126634886E-15, 0.4921259842519648542, -2.204724409448822975 ) ) ;
#565 = EDGE_CURVE ( 'NONE', #7376, #1597, #3596, .T. ) ;
#566 = DIRECTION ( 'NONE',  ( 0.000000000000000000, 0.000000000000000000, 1.000000000000000000 ) ) ;
#567 = CARTESIAN_POINT ( 'NONE',  ( 0.4332839536939404601, -0.9726683636255515353, -1.452651081959918544 ) ) ;
#568 = CARTESIAN_POINT ( 'NONE',  ( 0.3306743754077733355, 0.2557161625347751932, 0.1476377952755905942 ) ) ;
#569 = CONTEXT_DEPENDENT_SHAPE_REPRESENTATION ( #7163, #4969 ) ;
#570 = CARTESIAN_POINT ( 'NONE',  ( 0.3483227611829846637, -0.1704774416898499345, 0.2952755905511811330 ) ) ;
#571 = EDGE_CURVE ( 'NONE', #1688, #735, #1032, .T. ) ;
#572 = ORIENTED_EDGE ( 'NONE', *, *, #2208, .F. ) ;
#573 = CARTESIAN_POINT ( 'NONE',  ( -0.4375700189966297837, -1.070856827570679570, -1.565644132322242532 ) ) ;
#574 = CARTESIAN_POINT ( 'NONE',  ( -1.718248690375557255E-15, 0.4921259842519683514, -2.204724409448820754 ) ) ;
#575 = ORIENTED_EDGE ( 'NONE', *, *, #144, .F. ) ;
#576 = ORIENTED_EDGE ( 'NONE', *, *, #2847, .T. ) ;
#577 = DIRECTION ( 'NONE',  ( 0.3420201433256623291, 1.150791560227853228E-16, 0.9396926207859106484 ) ) ;
#578 = CARTESIAN_POINT ( 'NONE',  ( 1.968503937007874072, 0.000000000000000000, 0.4921259842519685179 ) ) ;
#579 =( BOUNDED_SURFACE ( )  B_SPLINE_SURFACE ( 3, 2, ( 
 ( #4765, #2351, #7019 ),
 ( #3619, #1771, #1123 ),
 ( #7095, #1812, #104 ),
 ( #4648, #4110, #4043 ),
 ( #6489, #5338, #6447 ),
 ( #2387, #2882, #4723 ),
 ( #1194, #3539, #1859 ),
 ( #5877, #1702, #639 ) ),
 .UNSPECIFIED., .F., .F., .F. ) 
 B_SPLINE_SURFACE_WITH_KNOTS ( ( 4, 2, 2, 4 ),
 ( 3, 3 ),
 ( 0.03552366018096265315, 0.03995354946645690575, 0.04216849410920403551, 0.04438343875195116528 ),
 ( 0.000000000000000000, 1.000000000000000000 ),
 .UNSPECIFIED. ) 
 GEOMETRIC_REPRESENTATION_ITEM ( )  RATIONAL_B_SPLINE_SURFACE ( (
 ( 1.000000000000000000, 0.8047780977832075244, 1.000000000000000000),
 ( 1.000000000000000000, 0.8123789484488428414, 1.000000000000000000),
 ( 1.000000000000000000, 0.8190677874188468932, 1.000000000000000000),
 ( 1.000000000000000000, 0.8191929099079664489, 1.000000000000000000),
 ( 1.000000000000000000, 0.8176081235728045460, 1.000000000000000000),
 ( 1.000000000000000000, 0.8122952617572927192, 1.000000000000000000),
 ( 1.000000000000000000, 0.8086306736854887989, 1.000000000000000000),
 ( 1.000000000000000000, 0.8047712637616463160, 1.000000000000000000) ) ) 
 REPRESENTATION_ITEM ( '' )  SURFACE ( )  );
#580 = EDGE_LOOP ( 'NONE', ( #4258, #6746, #2640, #4665, #5689, #5653, #4951 ) ) ;
#581 = DIRECTION ( 'NONE',  ( 0.000000000000000000, 0.000000000000000000, -1.000000000000000000 ) ) ;
#582 = B_SPLINE_CURVE_WITH_KNOTS ( 'NONE', 3,
 ( #6808, #3987, #473, #1036, #7411, #1561 ),
 .UNSPECIFIED., .F., .F.,
 ( 4, 2, 4 ),
 ( 2.380732026385019675E-07, 0.002190927868076661400, 0.004381617662950684777 ),
 .UNSPECIFIED. ) ;
#583 = AXIS2_PLACEMENT_3D ( 'NONE', #5101, #7419, #5821 ) ;
#584 = CARTESIAN_POINT ( 'NONE',  ( -1.003668447264492558, 0.4445641707282946831, -1.568529612473645862 ) ) ;
#585 = ORIENTED_EDGE ( 'NONE', *, *, #5580, .T. ) ;
#586 = ORIENTED_EDGE ( 'NONE', *, *, #2666, .T. ) ;
#587 = LINE ( 'NONE', #2905, #4789 ) ;
#588 = CARTESIAN_POINT ( 'NONE',  ( 0.3411158341578399145, -0.06121148758009550134, 0.3014953708557878698 ) ) ;
#589 = CARTESIAN_POINT ( 'NONE',  ( 18.30767084476541484, 38.73487850451988379, 54.41607747394844807 ) ) ;
#590 = CIRCLE ( 'NONE', #2658, 0.4921259842519685179 ) ;
#591 =( LENGTH_UNIT ( ) NAMED_UNIT ( * ) SI_UNIT ( $, .METRE. ) );
#592 = CARTESIAN_POINT ( 'NONE',  ( 0.3585568952266072751, -0.1763490727872195629, 0.3019338363380300039 ) ) ;
#593 = CARTESIAN_POINT ( 'NONE',  ( 0.3336175750056031841, 0.2273032555864666071, -0.1968503937007874127 ) ) ;
#594 = AXIS2_PLACEMENT_3D ( 'NONE', #7139, #4240, #4775 ) ;
#595 = ORIENTED_EDGE ( 'NONE', *, *, #2941, .T. ) ;
#596 = FACE_OUTER_BOUND ( 'NONE', #6777, .T. ) ;
#597 = CARTESIAN_POINT ( 'NONE',  ( 0.4700904924197906176, -0.8785537298370117432, -1.433776001880362250 ) ) ;
#598 = CIRCLE ( 'NONE', #108, 0.2952755905511810774 ) ;
#599 = CYLINDRICAL_SURFACE ( 'NONE', #4915, 0.4921259842519685179 ) ;
#600 = CARTESIAN_POINT ( 'NONE',  ( 0.000000000000000000, 0.000000000000000000, -0.4072677165354330331 ) ) ;
#601 = AXIS2_PLACEMENT_3D ( 'NONE', #3839, #2758, #6170 ) ;
#602 = FACE_OUTER_BOUND ( 'NONE', #6919, .T. ) ;
#603 = EDGE_CURVE ( 'NONE', #4444, #2106, #3724, .T. ) ;
#604 = EDGE_CURVE ( 'NONE', #5941, #7498, #3488, .T. ) ;
#605 = CARTESIAN_POINT ( 'NONE',  ( 0.4559220466128925953, -0.8989365377700702098, -1.445239289764781665 ) ) ;
#606 = CARTESIAN_POINT ( 'NONE',  ( 0.3581828924050324825, -0.1743168766271116221, -0.3019256869348722061 ) ) ;
#607 = DIRECTION ( 'NONE',  ( 0.000000000000000000, -1.000000000000000000, 2.095133389269358970E-15 ) ) ;
#608 = ORIENTED_EDGE ( 'NONE', *, *, #83, .T. ) ;
#609 = CIRCLE ( 'NONE', #2560, 0.2362204724409449341 ) ;
#610 = CARTESIAN_POINT ( 'NONE',  ( 0.4685039370078740717, 5.594759879304195485E-17, -0.4507874015748032370 ) ) ;
#611 = CARTESIAN_POINT ( 'NONE',  ( 0.000000000000000000, 0.000000000000000000, -0.4082677165354330340 ) ) ;
#612 = ORIENTED_EDGE ( 'NONE', *, *, #4824, .F. ) ;
#613 = EDGE_CURVE ( 'NONE', #5211, #5565, #6290, .T. ) ;
#614 = VERTEX_POINT ( 'NONE', #46 ) ;
#615 = ADVANCED_FACE ( 'NONE', ( #3566 ), #1657, .F. ) ;
#616 = CARTESIAN_POINT ( 'NONE',  ( 0.3997746709170348356, 0.000000000000000000, -0.4629062255509093782 ) ) ;
#617 = DIRECTION ( 'NONE',  ( 0.000000000000000000, 0.000000000000000000, -1.000000000000000000 ) ) ;
#618 = DIRECTION ( 'NONE',  ( 0.000000000000000000, -0.000000000000000000, 1.000000000000000000 ) ) ;
#619 = ORIENTED_EDGE ( 'NONE', *, *, #7330, .F. ) ;
#620 = CARTESIAN_POINT ( 'NONE',  ( 0.3426022948973417304, -0.05819196463765255456, -0.3015401604570891458 ) ) ;
#621 = CIRCLE ( 'NONE', #4896, 0.2066929133858267931 ) ;
#622 = DIRECTION ( 'NONE',  ( 0.8660254037844382635, 0.5000000000000006661, 0.000000000000000000 ) ) ;
#623 = ORIENTED_EDGE ( 'NONE', *, *, #4625, .F. ) ;
#624 = DIRECTION ( 'NONE',  ( 0.000000000000000000, 0.000000000000000000, 1.000000000000000000 ) ) ;
#625 = PLANE ( 'NONE',  #7312 ) ;
#626 = DIRECTION ( 'NONE',  ( 0.000000000000000000, 0.000000000000000000, -1.000000000000000000 ) ) ;
#627 = VECTOR ( 'NONE', #6886, 39.37007874015748143 ) ;
#628 = CARTESIAN_POINT ( 'NONE',  ( 0.3479985092864859020, -0.1192235226163089606, 0.3017044423212984494 ) ) ;
#629 = EDGE_LOOP ( 'NONE', ( #6063, #5640 ) ) ;
#630 = VERTEX_POINT ( 'NONE', #5218 ) ;
#631 = DIRECTION ( 'NONE',  ( -0.000000000000000000, -0.000000000000000000, 1.000000000000000000 ) ) ;
#632 = CARTESIAN_POINT ( 'NONE',  ( -0.9752011746066392428, -0.4617902729099834236, -1.554226146211527881 ) ) ;
#633 = AXIS2_PLACEMENT_3D ( 'NONE', #1426, #6154, #2659 ) ;
#634 = EDGE_LOOP ( 'NONE', ( #920, #6744 ) ) ;
#635 = AXIS2_PLACEMENT_3D ( 'NONE', #7232, #4794, #1411 ) ;
#636 = DIRECTION ( 'NONE',  ( -0.000000000000000000, 0.000000000000000000, -1.000000000000000000 ) ) ;
#637 = CIRCLE ( 'NONE', #3324, 0.4921259842519685179 ) ;
#638 = CARTESIAN_POINT ( 'NONE',  ( 3.198568410424924124, 2.407012729153881203, 0.000000000000000000 ) ) ;
#639 = CARTESIAN_POINT ( 'NONE',  ( 0.3585664987351884214, -0.1764010263750315499, -0.3019340449705225082 ) ) ;
#640 = AXIS2_PLACEMENT_3D ( 'NONE', #5169, #1024, #2176 ) ;
#641 = CARTESIAN_POINT ( 'NONE',  ( 0.5073440712904525585, -0.9696655408444868618, -1.367310953805774831 ) ) ;
#642 = CARTESIAN_POINT ( 'NONE',  ( -0.4882980771758828609, 0.9867934559254231131, -1.385219299502222112 ) ) ;
#643 = DIRECTION ( 'NONE',  ( 0.000000000000000000, -0.000000000000000000, 1.000000000000000000 ) ) ;
#644 = CONTEXT_DEPENDENT_SHAPE_REPRESENTATION ( #6533, #6483 ) ;
#645 = CARTESIAN_POINT ( 'NONE',  ( 21.65354330708661479, 0.000000000000000000, 0.000000000000000000 ) ) ;
#646 = DIRECTION ( 'NONE',  ( 1.000000000000000000, 0.000000000000000000, 0.000000000000000000 ) ) ;
#647 = CARTESIAN_POINT ( 'NONE',  ( 0.02637295201093703412, 0.1704774416898499345, 0.2952755905511810774 ) ) ;
#648 = DIRECTION ( 'NONE',  ( -1.000000000000000000, -8.881784197001252323E-16, -2.256009703088257329E-15 ) ) ;
#649 = ORIENTED_EDGE ( 'NONE', *, *, #1537, .F. ) ;
#650 = CIRCLE ( 'NONE', #1623, 0.9964144355006140374 ) ;
#651 = CARTESIAN_POINT ( 'NONE',  ( 1.968503937007874072, 0.000000000000000000, -0.2362204724409449619 ) ) ;
#652 = ADVANCED_FACE ( 'NONE', ( #1793, #4134, #5760 ), #3523, .T. ) ;
#653 = CARTESIAN_POINT ( 'NONE',  ( -0.5141614760841455301, -1.056523642887403414, -1.484898342931014081 ) ) ;
#654 = ORIENTED_EDGE ( 'NONE', *, *, #3315, .F. ) ;
#655 = VERTEX_POINT ( 'NONE', #4638 ) ;
#656 = PLANE ( 'NONE',  #1980 ) ;
#657 = CARTESIAN_POINT ( 'NONE',  ( 0.000000000000000000, 0.000000000000000000, -0.4082677165354330340 ) ) ;
#658 = ORIENTED_EDGE ( 'NONE', *, *, #3656, .T. ) ;
#659 = CARTESIAN_POINT ( 'NONE',  ( -0.3543307086614173040, -0.06891495372886451143, -0.002971448422589511792 ) ) ;
#660 = ADVANCED_FACE ( 'NONE', ( #2270 ), #492, .F. ) ;
#661 = EDGE_CURVE ( 'NONE', #4786, #3796, #1755, .T. ) ;
#662 = VERTEX_POINT ( 'NONE', #528 ) ;
#663 = AXIS2_PLACEMENT_3D ( 'NONE', #6765, #3244, #3283 ) ;
#664 = EDGE_CURVE ( 'NONE', #772, #6807, #4605, .T. ) ;
#665 = FACE_OUTER_BOUND ( 'NONE', #3589, .T. ) ;
#666 = CARTESIAN_POINT ( 'NONE',  ( -1.048552902599919401, -0.4330708661417353444, -1.573978973432617279 ) ) ;
#667 = DIRECTION ( 'NONE',  ( -1.000000000000000000, -0.000000000000000000, -4.625929269271482167E-15 ) ) ;
#668 = CARTESIAN_POINT ( 'NONE',  ( 0.3465690653189043013, 0.1180910924887165481, 0.2952755905511810774 ) ) ;
#669 = AXIS2_PLACEMENT_3D ( 'NONE', #1109, #7038, #4096 ) ;
#670 = VERTEX_POINT ( 'NONE', #6937 ) ;
#671 = DIRECTION ( 'NONE',  ( -0.000000000000000000, -0.000000000000000000, -1.000000000000000000 ) ) ;
#672 = DIRECTION ( 'NONE',  ( -0.000000000000000000, -0.000000000000000000, 1.000000000000000000 ) ) ;
#673 = APPLICATION_CONTEXT ( 'automotive_design' ) ;
#674 = ORIENTED_EDGE ( 'NONE', *, *, #6552, .T. ) ;
#675 =( NAMED_UNIT ( * ) PLANE_ANGLE_UNIT ( ) SI_UNIT ( $, .RADIAN. ) );
#676 = FACE_OUTER_BOUND ( 'NONE', #4781, .T. ) ;
#677 = CARTESIAN_POINT ( 'NONE',  ( -1.081428632361003839, 0.4470329974975731924, -1.553789141944099894 ) ) ;
#678 = CARTESIAN_POINT ( 'NONE',  ( 5.154746071126671174E-15, -0.4921259842519683514, -2.204724409448820754 ) ) ;
#679 = CARTESIAN_POINT ( 'NONE',  ( -2.834645669291338432, 0.000000000000000000, 0.000000000000000000 ) ) ;
#680 = PRODUCT_DEFINITION_CONTEXT ( 'detailed design', #1832, 'design' ) ;
#681 = CARTESIAN_POINT ( 'NONE',  ( -0.05817553349160984461, -0.3755582001340100895, -0.3942397458900140927 ) ) ;
#682 = CARTESIAN_POINT ( 'NONE',  ( 0.3543307086614173040, -0.1372236123666514263, -0.01398679180475823416 ) ) ;
#683 = CARTESIAN_POINT ( 'NONE',  ( 0.3336175750056032396, 0.2273032555864667459, 0.1968503937007873295 ) ) ;
#684 = CARTESIAN_POINT ( 'NONE',  ( 0.01171324505787554003, 0.3130206113228969356, 0.04838357847483527874 ) ) ;
#685 = FACE_OUTER_BOUND ( 'NONE', #2421, .T. ) ;
#686 = DIRECTION ( 'NONE',  ( -1.000000000000000000, 0.000000000000000000, 0.000000000000000000 ) ) ;
#687 = CARTESIAN_POINT ( 'NONE',  ( 0.000000000000000000, 0.2557161625347750267, 0.1476377952755908163 ) ) ;
#688 = EDGE_LOOP ( 'NONE', ( #319, #4284, #3558, #6790 ) ) ;
#689 = DIRECTION ( 'NONE',  ( -0.000000000000000000, -1.000000000000000000, -0.000000000000000000 ) ) ;
#690 = CARTESIAN_POINT ( 'NONE',  ( 0.000000000000000000, 0.000000000000000000, -1.515748031496062964 ) ) ;
#691 = FACE_OUTER_BOUND ( 'NONE', #2067, .T. ) ;
#692 = ORIENTED_EDGE ( 'NONE', *, *, #7245, .T. ) ;
#693 = CARTESIAN_POINT ( 'NONE',  ( 0.7499405322945513763, -0.03096673178975459240, 0.9837952645051013523 ) ) ;
#694 = ADVANCED_FACE ( 'NONE', ( #1693 ), #1141, .T. ) ;
#695 = CARTESIAN_POINT ( 'NONE',  ( 0.3543307086614173040, -0.2045729300278205376, -0.4082677165354330340 ) ) ;
#696 = EDGE_LOOP ( 'NONE', ( #3487, #218 ) ) ;
#697 = CARTESIAN_POINT ( 'NONE',  ( 0.3410249605999788325, -0.02903799983316278366, -0.3014927230551917026 ) ) ;
#698 = VERTEX_POINT ( 'NONE', #5829 ) ;
#699 = ORIENTED_EDGE ( 'NONE', *, *, #1392, .F. ) ;
#700 = CARTESIAN_POINT ( 'NONE',  ( 0.4339190921229452713, -0.9541934910893031807, -1.456692913385827071 ) ) ;
#701 = EDGE_CURVE ( 'NONE', #3513, #6455, #587, .T. ) ;
#702 = EDGE_CURVE ( 'NONE', #3366, #1329, #5656, .T. ) ;
#703 = APPLICATION_PROTOCOL_DEFINITION ( 'draft international standard', 'automotive_design', 1998, #3952 ) ;
#704 = CARTESIAN_POINT ( 'NONE',  ( 0.3442721343065135997, 0.1485366976410457951, 0.2952755905511810774 ) ) ;
#705 =( GEOMETRIC_REPRESENTATION_CONTEXT ( 3 ) GLOBAL_UNCERTAINTY_ASSIGNED_CONTEXT ( ( #302 ) ) GLOBAL_UNIT_ASSIGNED_CONTEXT ( ( #3871, #7455, #7381 ) ) REPRESENTATION_CONTEXT ( 'NONE', 'WORKASPACE' ) );
#706 = EDGE_CURVE ( 'NONE', #2864, #1140, #22, .T. ) ;
#707 = CARTESIAN_POINT ( 'NONE',  ( 0.000000000000000000, 0.2559055118110236116, -0.2362204724409449341 ) ) ;
#708 = DIRECTION ( 'NONE',  ( 0.000000000000000000, 0.000000000000000000, 1.000000000000000000 ) ) ;
#709 = VERTEX_POINT ( 'NONE', #5413 ) ;
#710 = TOROIDAL_SURFACE ( 'NONE', #4988, 1.043121362164705745, 0.05905511811023622659 ) ;
#711 = EDGE_CURVE ( 'NONE', #3346, #4166, #2412, .T. ) ;
#712 = CARTESIAN_POINT ( 'NONE',  ( 0.3487102105009288744, -0.3201373431253433655, -0.04891434758976972302 ) ) ;
#713 = CARTESIAN_POINT ( 'NONE',  ( 0.000000000000000000, 0.000000000000000000, 0.000000000000000000 ) ) ;
#714 = CARTESIAN_POINT ( 'NONE',  ( -1.078368813366572310, 0.4878045971889936605, -1.510181706589752482 ) ) ;
#715 = B_SPLINE_CURVE_WITH_KNOTS ( 'NONE', 3,
 ( #570, #5234, #1661, #2317, #6988, #4119 ),
 .UNSPECIFIED., .F., .F.,
 ( 4, 2, 4 ),
 ( 0.000000000000000000, 0.0001677595217559109278, 0.0003355190435118218556 ),
 .UNSPECIFIED. ) ;
#716 = LINE ( 'NONE', #1979, #7122 ) ;
#717 = CARTESIAN_POINT ( 'NONE',  ( -0.1771653543307089018, -0.3068593950417300986, -0.4082677165354330340 ) ) ;
#718 = CARTESIAN_POINT ( 'NONE',  ( 0.4663806185493042933, -0.8833138556570224731, -1.436938405272258246 ) ) ;
#719 = CARTESIAN_POINT ( 'NONE',  ( 0.3483227611829848303, 0.3409548833797004797, 0.000000000000000000 ) ) ;
#720 = AXIS2_PLACEMENT_3D ( 'NONE', #645, #4729, #2481 ) ;
#721 = FACE_OUTER_BOUND ( 'NONE', #7140, .T. ) ;
#722 = CARTESIAN_POINT ( 'NONE',  ( 0.000000000000000000, 0.000000000000000000, -0.2952755905511810774 ) ) ;
#723 = CARTESIAN_POINT ( 'NONE',  ( 2.755905511811024056, 0.000000000000000000, 0.000000000000000000 ) ) ;
#724 = CARTESIAN_POINT ( 'NONE',  ( 0.3543307086614173040, -0.1372236123666513430, -0.3942809247306748865 ) ) ;
#725 = VERTEX_POINT ( 'NONE', #1380 ) ;
#726 = CARTESIAN_POINT ( 'NONE',  ( 0.4685039370078740717, 0.1704774416898497680, -0.2952755905511810774 ) ) ;
#727 = DIRECTION ( 'NONE',  ( 0.000000000000000000, 1.000000000000000000, 2.256009703088257329E-15 ) ) ;
#728 = ORIENTED_EDGE ( 'NONE', *, *, #3375, .F. ) ;
#729 = LINE ( 'NONE', #768, #2227 ) ;
#730 = AXIS2_PLACEMENT_3D ( 'NONE', #3349, #2774, #2203 ) ;
#731 = CARTESIAN_POINT ( 'NONE',  ( 1.968503937007874072, 0.000000000000000000, 0.9842519685039370358 ) ) ;
#732 = CARTESIAN_POINT ( 'NONE',  ( 1.968503937007874072, 0.000000000000000000, 0.000000000000000000 ) ) ;
#733 = VERTEX_POINT ( 'NONE', #5947 ) ;
#734 = LINE ( 'NONE', #3056, #2724 ) ;
#735 = VERTEX_POINT ( 'NONE', #2004 ) ;
#736 = EDGE_LOOP ( 'NONE', ( #7405, #7185, #280, #6307 ) ) ;
#737 = DIRECTION ( 'NONE',  ( -0.000000000000000000, -0.000000000000000000, 1.000000000000000000 ) ) ;
#738 = CARTESIAN_POINT ( 'NONE',  ( 0.3459468362671123676, -0.1200707489736706907, 0.2952755905511811885 ) ) ;
#739 = APPLICATION_PROTOCOL_DEFINITION ( 'draft international standard', 'automotive_design', 1998, #1289 ) ;
#740 = SURFACE_STYLE_FILL_AREA ( #1797 ) ;
#741 = ORIENTED_EDGE ( 'NONE', *, *, #3231, .F. ) ;
#742 = CARTESIAN_POINT ( 'NONE',  ( -1.048552902599919401, -0.4330708661417353444, -1.573978973432617279 ) ) ;
#743 = DIRECTION ( 'NONE',  ( 0.000000000000000000, 0.000000000000000000, -1.000000000000000000 ) ) ;
#744 = EDGE_CURVE ( 'NONE', #6545, #6588, #776, .T. ) ;
#745 = PRODUCT_DEFINITION_SHAPE ( 'NONE', 'NONE',  #7538 ) ;
#746 = CARTESIAN_POINT ( 'NONE',  ( 0.01834252172841674411, -0.3270457701237520221, -0.02409129084753309710 ) ) ;
#747 = CARTESIAN_POINT ( 'NONE',  ( -1.070877820178679052, 0.4996352642496060814, -1.498503547059352181 ) ) ;
#748 = CIRCLE ( 'NONE', #7336, 0.2952755905511810774 ) ;
#749 = LINE ( 'NONE', #5426, #4924 ) ;
#750 = LINE ( 'NONE', #6040, #5742 ) ;
#751 = ADVANCED_FACE ( 'NONE', ( #1841 ), #84, .F. ) ;
#752 = ADVANCED_FACE ( 'NONE', ( #814 ), #1606, .F. ) ;
#753 = VECTOR ( 'NONE', #7293, 39.37007874015748143 ) ;
#754 = PRODUCT_DEFINITION_CONTEXT ( 'detailed design', #2240, 'design' ) ;
#755 = DIRECTION ( 'NONE',  ( 0.000000000000000000, 0.000000000000000000, 1.000000000000000000 ) ) ;
#756 = CIRCLE ( 'NONE', #6979, 0.2362204724409449341 ) ;
#757 = CARTESIAN_POINT ( 'NONE',  ( 2.755905511811024056, 1.496062992125984259, 0.000000000000000000 ) ) ;
#758 = CONTEXT_DEPENDENT_SHAPE_REPRESENTATION ( #6421, #2517 ) ;
#759 = CARTESIAN_POINT ( 'NONE',  ( 0.01834252172841645614, 0.3270457701237517445, 0.02409129084753309363 ) ) ;
#760 = DIRECTION ( 'NONE',  ( 0.000000000000000000, 1.000000000000000000, 0.000000000000000000 ) ) ;
#761 = DIRECTION ( 'NONE',  ( -1.000000000000000000, 0.000000000000000000, 0.000000000000000000 ) ) ;
#762 = CARTESIAN_POINT ( 'NONE',  ( 1.718248690375545225E-15, -0.4921259842519648542, -2.204724409448822975 ) ) ;
#763 = ORIENTED_EDGE ( 'NONE', *, *, #1199, .T. ) ;
#764 = CARTESIAN_POINT ( 'NONE',  ( 1.611653543307086212, 0.000000000000000000, 0.2362204724409449064 ) ) ;
#765 = CARTESIAN_POINT ( 'NONE',  ( 3.027559055118110187, 2.660472849486257786E-17, -0.1982677165354330695 ) ) ;
#766 = VECTOR ( 'NONE', #2837, 39.37007874015748143 ) ;
#767 = ORIENTED_EDGE ( 'NONE', *, *, #2252, .F. ) ;
#768 = CARTESIAN_POINT ( 'NONE',  ( -2.834645669291338432, 0.000000000000000000, 0.4724409448818898127 ) ) ;
#769 = CARTESIAN_POINT ( 'NONE',  ( 21.65354330708661479, 0.000000000000000000, 0.000000000000000000 ) ) ;
#770 = AXIS2_PLACEMENT_3D ( 'NONE', #6990, #1284, #6503 ) ;
#771 = CARTESIAN_POINT ( 'NONE',  ( 0.01841426102874288775, 0.1429077274040485568, 0.2952755905511811330 ) ) ;
#772 = VERTEX_POINT ( 'NONE', #129 ) ;
#773 = CARTESIAN_POINT ( 'NONE',  ( 0.3391216574608371670, 0.3159523085418723398, -0.04330572993916122215 ) ) ;
#774 = ORIENTED_EDGE ( 'NONE', *, *, #4146, .T. ) ;
#775 = ORIENTED_EDGE ( 'NONE', *, *, #256, .T. ) ;
#776 = LINE ( 'NONE', #5984, #154 ) ;
#777 = PRODUCT_CONTEXT ( 'NONE', #915, 'mechanical' ) ;
#778 = DIRECTION ( 'NONE',  ( -1.000000000000000000, 0.000000000000000000, 0.000000000000000000 ) ) ;
#779 = CARTESIAN_POINT ( 'NONE',  ( 0.3531511627980717938, 0.3349346966101464096, 0.02350890366534340997 ) ) ;
#780 = ORIENTED_EDGE ( 'NONE', *, *, #4918, .T. ) ;
#781 = VERTEX_POINT ( 'NONE', #3604 ) ;
#782 = AXIS2_PLACEMENT_3D ( 'NONE', #1020, #6876, #6486 ) ;
#783 = PRESENTATION_LAYER_ASSIGNMENT (  '', '', ( #5795 ) ) ;
#784 = CARTESIAN_POINT ( 'NONE',  ( 0.000000000000000000, 0.000000000000000000, 0.000000000000000000 ) ) ;
#785 = SHAPE_REPRESENTATION ( 'Base', ( #5166 ), #4425 ) ;
#786 = ORIENTED_EDGE ( 'NONE', *, *, #5010, .F. ) ;
#787 = PRODUCT_DEFINITION ( 'UNKNOWN', '', #6798, #7097 ) ;
#788 = CARTESIAN_POINT ( 'NONE',  ( -0.4388996395293570107, 0.9346850374427959629, -1.455943645409048637 ) ) ;
#789 = CARTESIAN_POINT ( 'NONE',  ( 0.4713813068963902952, -1.084813395429188088, -1.526966363676887317 ) ) ;
#790 = CARTESIAN_POINT ( 'NONE',  ( 1.207998888640173130, 0.07614347099379424610, -0.9813305615101511892 ) ) ;
#791 = DIRECTION ( 'NONE',  ( 1.000000000000000000, 0.000000000000000000, 0.000000000000000000 ) ) ;
#792 = DIRECTION ( 'NONE',  ( -0.000000000000000000, -0.000000000000000000, 1.000000000000000000 ) ) ;
#793 = EDGE_CURVE ( 'NONE', #1455, #4636, #5492, .T. ) ;
#794 = ADVANCED_FACE ( 'NONE', ( #250 ), #211, .F. ) ;
#795 = CARTESIAN_POINT ( 'NONE',  ( 21.65354330708661479, 6.026805113914139867E-17, -0.4921259842519685179 ) ) ;
#796 = LINE ( 'NONE', #5434, #3412 ) ;
#797 = FACE_OUTER_BOUND ( 'NONE', #6325, .T. ) ;
#798 = CARTESIAN_POINT ( 'NONE',  ( 1.170506159394721758E-17, 0.02884736746562922144, 0.2952755905511810774 ) ) ;
#799 = CARTESIAN_POINT ( 'NONE',  ( 0.3997746709170348356, 0.000000000000000000, -0.4629062255509093782 ) ) ;
#800 = EDGE_LOOP ( 'NONE', ( #7228, #4213, #2502, #2646 ) ) ;
#801 = CARTESIAN_POINT ( 'NONE',  ( 0.1771653543307089296, -0.3068593950417301541, -0.4082677165354330340 ) ) ;
#802 = ADVANCED_FACE ( 'NONE', ( #665 ), #2984, .F. ) ;
#803 = CARTESIAN_POINT ( 'NONE',  ( 0.000000000000000000, 0.000000000000000000, -0.2952755905511810774 ) ) ;
#804 = CARTESIAN_POINT ( 'NONE',  ( 0.01832242175888446414, 0.1844213691142423395, 0.2711239997950803393 ) ) ;
#805 = CARTESIAN_POINT ( 'NONE',  ( 0.000000000000000000, 0.000000000000000000, 0.000000000000000000 ) ) ;
#806 = DIRECTION ( 'NONE',  ( -0.000000000000000000, -0.000000000000000000, -1.000000000000000000 ) ) ;
#807 = ADVANCED_FACE ( 'NONE', ( #6519 ), #1567, .F. ) ;
#808 = CARTESIAN_POINT ( 'NONE',  ( 0.002549129251874865387, 0.05807386165059042621, 0.2952755905511811330 ) ) ;
#809 = EDGE_LOOP ( 'NONE', ( #524, #964, #2532, #4873 ) ) ;
#810 = CARTESIAN_POINT ( 'NONE',  ( 0.3409812221349237671, 0.2467127425963012433, -0.1756638922268426994 ) ) ;
#811 = VERTEX_POINT ( 'NONE', #3253 ) ;
#812 = PRODUCT_DEFINITION_SHAPE ( 'NONE', 'NONE',  #7541 ) ;
#813 = VERTEX_POINT ( 'NONE', #925 ) ;
#814 = FACE_OUTER_BOUND ( 'NONE', #1293, .T. ) ;
#815 =( BOUNDED_SURFACE ( )  B_SPLINE_SURFACE ( 3, 2, ( 
 ( #7486, #6848, #2145 ),
 ( #1604, #2823, #6278 ),
 ( #5176, #998, #3908 ),
 ( #4479, #5135, #3332 ),
 ( #2752, #5093, #6921 ),
 ( #5783, #2184, #435 ),
 ( #1065, #7447, #2260 ),
 ( #2223, #4518, #3950 ) ),
 .UNSPECIFIED., .F., .F., .F. ) 
 B_SPLINE_SURFACE_WITH_KNOTS ( ( 4, 2, 2, 4 ),
 ( 3, 3 ),
 ( 0.03551798592901333346, 0.03994769179990642627, 0.04216254473535296921, 0.04437739767079951908 ),
 ( 0.000000000000000000, 1.000000000000000000 ),
 .UNSPECIFIED. ) 
 GEOMETRIC_REPRESENTATION_ITEM ( )  RATIONAL_B_SPLINE_SURFACE ( (
 ( 1.000000000000000000, 0.8047781103519390244, 1.000000000000000000),
 ( 1.000000000000000000, 0.8123785826175446978, 1.000000000000000000),
 ( 1.000000000000000000, 0.8190671539027887249, 1.000000000000000000),
 ( 1.000000000000000000, 0.8191932076453414258, 1.000000000000000000),
 ( 1.000000000000000000, 0.8176085094066379844, 1.000000000000000000),
 ( 1.000000000000000000, 0.8122955484014008354, 1.000000000000000000),
 ( 1.000000000000000000, 0.8086308001280824165, 1.000000000000000000),
 ( 1.000000000000000000, 0.8047712537969731184, 1.000000000000000000) ) ) 
 REPRESENTATION_ITEM ( '' )  SURFACE ( )  );
#816 =( REPRESENTATION_RELATIONSHIP ('NONE','NONE', #303, #1552 ) REPRESENTATION_RELATIONSHIP_WITH_TRANSFORMATION ( #6805 )SHAPE_REPRESENTATION_RELATIONSHIP( ) );
#817 = LINE ( 'NONE', #7304, #1421 ) ;
#818 = CARTESIAN_POINT ( 'NONE',  ( 0.9609181420092369752, -0.5141614760841358711, -1.361499588670819216 ) ) ;
#819 = ORIENTED_EDGE ( 'NONE', *, *, #5100, .F. ) ;
#820 = LINE ( 'NONE', #3731, #6144 ) ;
#821 = ORIENTED_EDGE ( 'NONE', *, *, #2617, .T. ) ;
#822 = DIRECTION ( 'NONE',  ( -2.312579046053608732E-29, 2.207829878515936732E-15, 1.000000000000000000 ) ) ;
#823 = ORIENTED_EDGE ( 'NONE', *, *, #2569, .F. ) ;
#824 =( NAMED_UNIT ( * ) SI_UNIT ( $, .STERADIAN. ) SOLID_ANGLE_UNIT ( ) );
#825 = CIRCLE ( 'NONE', #3885, 0.2362204724409449341 ) ;
#826 = DIRECTION ( 'NONE',  ( -1.000000000000000000, -0.000000000000000000, -0.000000000000000000 ) ) ;
#827 = AXIS2_PLACEMENT_3D ( 'NONE', #4003, #1086, #6905 ) ;
#828 = CARTESIAN_POINT ( 'NONE',  ( 0.9763767025864577009, -0.2362177056199707692, -0.9554858099749828915 ) ) ;
#829 = DIRECTION ( 'NONE',  ( -1.000000000000000000, 0.000000000000000000, -0.000000000000000000 ) ) ;
#830 = VECTOR ( 'NONE', #949, 39.37007874015748143 ) ;
#831 = DIRECTION ( 'NONE',  ( -1.000000000000000000, -0.000000000000000000, -0.000000000000000000 ) ) ;
#832 = DIRECTION ( 'NONE',  ( -1.000000000000000000, 0.000000000000000000, 0.000000000000000000 ) ) ;
#833 = CARTESIAN_POINT ( 'NONE',  ( 0.8884022185686345496, -0.4627504720074674949, -1.439912370850673806 ) ) ;
#834 = CARTESIAN_POINT ( 'NONE',  ( 0.01168997831664888090, -0.3129651733100090039, 0.04847959992982862204 ) ) ;
#835 = VECTOR ( 'NONE', #3623, 39.37007874015748143 ) ;
#836 = CARTESIAN_POINT ( 'NONE',  ( 0.3485373078438442351, 0.3194486952732363827, 0.05009812457233156491 ) ) ;
#837 = CARTESIAN_POINT ( 'NONE',  ( 1.023371766162640473, 0.4368380215374228492, -1.573834103987475475 ) ) ;
#838 = DIRECTION ( 'NONE',  ( -0.000000000000000000, -1.000000000000000000, -0.000000000000000000 ) ) ;
#839 = ORIENTED_EDGE ( 'NONE', *, *, #6725, .F. ) ;
#840 = CARTESIAN_POINT ( 'NONE',  ( 0.3432736861146661322, -0.1846838951640041859, 0.2706692913385828625 ) ) ;
#841 = CARTESIAN_POINT ( 'NONE',  ( -0.4996355910473242457, 1.070877566692229221, -1.498503231159225457 ) ) ;
#842 = EDGE_CURVE ( 'NONE', #3073, #450, #2024, .T. ) ;
#843 = ORIENTED_EDGE ( 'NONE', *, *, #3133, .F. ) ;
#844 = AXIS2_PLACEMENT_3D ( 'NONE', #5552, #1023, #6983 ) ;
#845 = DIRECTION ( 'NONE',  ( 0.000000000000000000, 1.000000000000000000, 0.000000000000000000 ) ) ;
#846 = CARTESIAN_POINT ( 'NONE',  ( 0.3459458835994366765, 0.1200656956960832605, -0.2952755905511810774 ) ) ;
#847 = CARTESIAN_POINT ( 'NONE',  ( 0.4837911690062421388, 1.080458355692614614, -1.514208178040841180 ) ) ;
#848 = ORIENTED_EDGE ( 'NONE', *, *, #702, .T. ) ;
#849 = TOROIDAL_SURFACE ( 'NONE', #4129, 1.223643328182682621, 0.05905511811023622659 ) ;
#850 = DIRECTION ( 'NONE',  ( -1.000000000000000000, -0.000000000000000000, -0.000000000000000000 ) ) ;
#851 = EDGE_CURVE ( 'NONE', #7286, #3362, #1476, .T. ) ;
#852 = ADVANCED_FACE ( 'NONE', ( #6737 ), #5603, .F. ) ;
#853 = EDGE_LOOP ( 'NONE', ( #3099, #6673, #4483, #2834, #4737 ) ) ;
#854 = CARTESIAN_POINT ( 'NONE',  ( 0.01836325778988931109, -0.1427310470019619582, -0.2952755905511810774 ) ) ;
#855 = AXIS2_PLACEMENT_3D ( 'NONE', #7211, #5510, #4158 ) ;
#856 = CARTESIAN_POINT ( 'NONE',  ( 0.000000000000000000, 0.000000000000000000, 0.1188976377952756375 ) ) ;
#857 = CARTESIAN_POINT ( 'NONE',  ( 0.3409812221349194372, 0.2754857644942527717, 0.1258275564122752488 ) ) ;
#858 = EDGE_LOOP ( 'NONE', ( #6817, #174, #897, #1527, #4829, #1104 ) ) ;
#859 = CARTESIAN_POINT ( 'NONE',  ( 0.3574299024618897702, 0.3465649303883613364, 6.884133197150707104E-16 ) ) ;
#860 = ORIENTED_EDGE ( 'NONE', *, *, #6926, .T. ) ;
#861 = AXIS2_PLACEMENT_3D ( 'NONE', #4913, #7238, #6321 ) ;
#862 = FACE_OUTER_BOUND ( 'NONE', #1840, .T. ) ;
#863 = ORIENTED_EDGE ( 'NONE', *, *, #382, .F. ) ;
#864 = DIRECTION ( 'NONE',  ( 0.000000000000000000, 0.000000000000000000, 1.000000000000000000 ) ) ;
#865 =( LENGTH_UNIT ( ) NAMED_UNIT ( * ) SI_UNIT ( $, .METRE. ) );
#866 = DIRECTION ( 'NONE',  ( -0.000000000000000000, -1.000000000000000000, -0.000000000000000000 ) ) ;
#867 = AXIS2_PLACEMENT_3D ( 'NONE', #4206, #5973, #1163 ) ;
#868 = DIRECTION ( 'NONE',  ( 0.000000000000000000, 0.000000000000000000, -1.000000000000000000 ) ) ;
#869 = LINE ( 'NONE', #6839, #2602 ) ;
#870 = CARTESIAN_POINT ( 'NONE',  ( 0.3410425348215777031, 0.2759054741781710729, -0.1251041708914593098 ) ) ;
#871 = DIRECTION ( 'NONE',  ( -0.000000000000000000, -1.000000000000000000, -0.000000000000000000 ) ) ;
#872 = DIRECTION ( 'NONE',  ( 1.000000000000000000, 0.000000000000000000, 0.000000000000000000 ) ) ;
#873 = ORIENTED_EDGE ( 'NONE', *, *, #5995, .T. ) ;
#874 = PRODUCT_DEFINITION_SHAPE ( 'NONE', 'NONE',  #7519 ) ;
#875 = CARTESIAN_POINT ( 'NONE',  ( -0.9984401429152555130, 0.4637690556582312329, -1.410743228759549828 ) ) ;
#876 = CARTESIAN_POINT ( 'NONE',  ( -0.4713815370807409866, 1.084813347358863700, -1.526966122205014820 ) ) ;
#877 = AXIS2_PLACEMENT_3D ( 'NONE', #2744, #465, #539 ) ;
#878 = ORIENTED_EDGE ( 'NONE', *, *, #1482, .F. ) ;
#879 =( GEOMETRIC_REPRESENTATION_CONTEXT ( 3 ) GLOBAL_UNCERTAINTY_ASSIGNED_CONTEXT ( ( #4809 ) ) GLOBAL_UNIT_ASSIGNED_CONTEXT ( ( #5297, #1854, #6527 ) ) REPRESENTATION_CONTEXT ( 'NONE', 'WORKASPACE' ) );
#880 = CARTESIAN_POINT ( 'NONE',  ( 7.874015748031496287, 0.000000000000000000, 0.000000000000000000 ) ) ;
#881 = DIRECTION ( 'NONE',  ( 0.000000000000000000, 0.000000000000000000, -1.000000000000000000 ) ) ;
#882 = EDGE_CURVE ( 'NONE', #2163, #1804, #285, .T. ) ;
#883 = CARTESIAN_POINT ( 'NONE',  ( 0.4508657589754702655, 1.083410700381145508, -1.549345605342071774 ) ) ;
#884 = ORIENTED_EDGE ( 'NONE', *, *, #2364, .F. ) ;
#885 = AXIS2_PLACEMENT_3D ( 'NONE', #4491, #6900, #4130 ) ;
#886 = DIRECTION ( 'NONE',  ( 1.000000000000000000, 1.049299683535328711E-14, 0.000000000000000000 ) ) ;
#887 = ORIENTED_EDGE ( 'NONE', *, *, #2928, .F. ) ;
#888 = ORIENTED_EDGE ( 'NONE', *, *, #7418, .T. ) ;
#889 = AXIS2_PLACEMENT_3D ( 'NONE', #5715, #3333, #2261 ) ;
#890 = CARTESIAN_POINT ( 'NONE',  ( 0.02637295201093751290, -0.3409548833797009237, -9.138209691400258722E-18 ) ) ;
#891 = EDGE_CURVE ( 'NONE', #6362, #4753, #7466, .T. ) ;
#892 = CARTESIAN_POINT ( 'NONE',  ( 0.3543307086614173596, -0.2045729300278204543, -0.03164754241312491001 ) ) ;
#893 = ADVANCED_FACE ( 'NONE', ( #1524 ), #6865, .T. ) ;
#894 = DIRECTION ( 'NONE',  ( -1.000000000000000000, -1.047444401652940007E-14, -6.779428194327236205E-32 ) ) ;
#895 = ORIENTED_EDGE ( 'NONE', *, *, #1257, .T. ) ;
#896 = CARTESIAN_POINT ( 'NONE',  ( 0.7836514762968587178, 0.1249763776241986785, 0.9763066675542205752 ) ) ;
#897 = ORIENTED_EDGE ( 'NONE', *, *, #2246, .F. ) ;
#898 = CIRCLE ( 'NONE', #5179, 0.3543307086614173596 ) ;
#899 = CARTESIAN_POINT ( 'NONE',  ( 2.755905511811024056, 1.496062992125984259, -0.7480314960629921295 ) ) ;
#900 = EDGE_CURVE ( 'NONE', #6925, #7325, #6669, .T. ) ;
#901 = EDGE_LOOP ( 'NONE', ( #6061, #332, #5893, #4548 ) ) ;
#902 = ORIENTED_EDGE ( 'NONE', *, *, #6171, .F. ) ;
#903 = CARTESIAN_POINT ( 'NONE',  ( 25.88474923092189783, 33.59468125523034843, 51.90562702829911501 ) ) ;
#904 = CYLINDRICAL_SURFACE ( 'NONE', #5507, 0.4921259842519685179 ) ;
#905 = DIRECTION ( 'NONE',  ( 1.000000000000000000, 0.000000000000000000, -0.000000000000000000 ) ) ;
#906 = FILL_AREA_STYLE_COLOUR ( '', #1504 ) ;
#907 = AXIS2_PLACEMENT_3D ( 'NONE', #6219, #3810, #4309 ) ;
#908 = CARTESIAN_POINT ( 'NONE',  ( 0.000000000000000000, 0.000000000000000000, -1.574803149606299302 ) ) ;
#909 = LINE ( 'NONE', #5549, #7094 ) ;
#910 = CARTESIAN_POINT ( 'NONE',  ( 0.4663632139996677362, 0.8833361873720626534, -1.436953241411902837 ) ) ;
#911 = CARTESIAN_POINT ( 'NONE',  ( 0.000000000000000000, 0.000000000000000000, -3.582716535433073002 ) ) ;
#912 = CARTESIAN_POINT ( 'NONE',  ( 0.01171324505787554003, 0.3130206113228969356, 0.04838357847483527874 ) ) ;
#913 = VERTEX_POINT ( 'NONE', #2606 ) ;
#914 = CARTESIAN_POINT ( 'NONE',  ( -1.861696953619914682E-15, 0.000000000000000000, -1.361499588670820771 ) ) ;
#915 = APPLICATION_CONTEXT ( 'automotive_design' ) ;
#916 = CARTESIAN_POINT ( 'NONE',  ( 0.01168997831664865018, 0.3129651733100085598, -0.04847959992982851796 ) ) ;
#917 = CARTESIAN_POINT ( 'NONE',  ( 0.3391211773724056577, 0.1204696997606904962, -0.2952755905511810774 ) ) ;
#918 = APPLICATION_PROTOCOL_DEFINITION ( 'draft international standard', 'automotive_design', 1998, #438 ) ;
#919 = CARTESIAN_POINT ( 'NONE',  ( 0.000000000000000000, 0.000000000000000000, 0.000000000000000000 ) ) ;
#920 = ORIENTED_EDGE ( 'NONE', *, *, #6725, .T. ) ;
#921 = CARTESIAN_POINT ( 'NONE',  ( 0.3565325103478086399, 0.3440765519545058160, 0.005406888575954027845 ) ) ;
#922 = ORIENTED_EDGE ( 'NONE', *, *, #3553, .T. ) ;
#923 = EDGE_CURVE ( 'NONE', #1513, #1261, #5686, .T. ) ;
#924 = ORIENTED_EDGE ( 'NONE', *, *, #2848, .T. ) ;
#925 = CARTESIAN_POINT ( 'NONE',  ( 0.000000000000000000, 1.496062992125984259, -0.7480314960629921295 ) ) ;
#926 = CARTESIAN_POINT ( 'NONE',  ( 1.968503937007874072, 0.000000000000000000, 0.9842519685039370358 ) ) ;
#927 = ORIENTED_EDGE ( 'NONE', *, *, #387, .T. ) ;
#928 = CARTESIAN_POINT ( 'NONE',  ( -0.4330708661417287941, 0.000000000000000000, -2.204724409448822975 ) ) ;
#929 = VERTEX_POINT ( 'NONE', #3762 ) ;
#930 = CARTESIAN_POINT ( 'NONE',  ( 1.045446081760740942, 0.2286795840550674142, 0.9573229298165720769 ) ) ;
#931 = VERTEX_POINT ( 'NONE', #4484 ) ;
#932 = CARTESIAN_POINT ( 'NONE',  ( 0.3391216574609289269, 0.1954800165277119361, 0.2519698606119610829 ) ) ;
#933 = CARTESIAN_POINT ( 'NONE',  ( 0.000000000000000000, 0.000000000000000000, 0.7480314960629921295 ) ) ;
#934 = ORIENTED_EDGE ( 'NONE', *, *, #5286, .F. ) ;
#935 = PRODUCT_DEFINITION_FORMATION_WITH_SPECIFIED_SOURCE ( 'ANY', '', #3614, .NOT_KNOWN. ) ;
#936 = EDGE_CURVE ( 'NONE', #5718, #4898, #5884, .T. ) ;
#937 = ADVANCED_FACE ( 'NONE', ( #2757 ), #4947, .T. ) ;
#938 = B_SPLINE_CURVE_WITH_KNOTS ( 'NONE', 3,
 ( #3301, #6822, #700, #7081 ),
 .UNSPECIFIED., .F., .F.,
 ( 4, 4 ),
 ( 0.000000000000000000, 0.0004815725036528474990 ),
 .UNSPECIFIED. ) ;
#939 = B_SPLINE_CURVE_WITH_KNOTS ( 'NONE', 3,
 ( #485, #5690, #2265, #6287, #5309, #2800, #7383, #5886, #5184 ),
 .UNSPECIFIED., .F., .F.,
 ( 4, 2, 1, 2, 4 ),
 ( 0.000000000000000000, 0.002165063509461098799, 0.004330127018922199332, 0.006495190528383298564, 0.008660254037844398664 ),
 .UNSPECIFIED. ) ;
#940 = DIRECTION ( 'NONE',  ( 0.4978050506594157154, 0.8672889550420763705, 5.264840435781089266E-31 ) ) ;
#941 = PRODUCT_DEFINITION_SHAPE ( 'NONE', 'NONE',  #7550 ) ;
#942 = DIRECTION ( 'NONE',  ( 0.000000000000000000, 1.000000000000000000, 0.000000000000000000 ) ) ;
#943 = EDGE_CURVE ( 'NONE', #4878, #913, #2079, .T. ) ;
#944 = CYLINDRICAL_SURFACE ( 'NONE', #2080, 0.4724409448818896462 ) ;
#945 = CARTESIAN_POINT ( 'NONE',  ( 0.000000000000000000, 0.000000000000000000, -2.204724409448820754 ) ) ;
#946 = EDGE_CURVE ( 'NONE', #1068, #3331, #4296, .T. ) ;
#947 = ADVANCED_FACE ( 'NONE', ( #2325 ), #1113, .T. ) ;
#948 = CARTESIAN_POINT ( 'NONE',  ( 1.968503937007874072, 6.026805113914139867E-17, -0.4921259842519685179 ) ) ;
#949 = DIRECTION ( 'NONE',  ( -0.000000000000000000, -0.000000000000000000, -1.000000000000000000 ) ) ;
#950 = CARTESIAN_POINT ( 'NONE',  ( 0.9755734897585840448, 0.4619485889667721001, -1.553989674004691901 ) ) ;
#951 = VERTEX_POINT ( 'NONE', #1748 ) ;
#952 = B_SPLINE_CURVE_WITH_KNOTS ( 'NONE', 3,
 ( #1363, #798, #4160, #2396, #69, #647 ),
 .UNSPECIFIED., .F., .F.,
 ( 4, 2, 4 ),
 ( 0.01227927579290655560, 0.01447189347357576844, 0.01666451115424498128 ),
 .UNSPECIFIED. ) ;
#953 = CIRCLE ( 'NONE', #4610, 1.174991162294038771 ) ;
#954 = CARTESIAN_POINT ( 'NONE',  ( 0.000000000000000000, 0.3409548833797004797, 2.164902785881980513E-17 ) ) ;
#955 = ORIENTED_EDGE ( 'NONE', *, *, #1246, .T. ) ;
#956 = DIRECTION ( 'NONE',  ( -1.000000000000000000, -0.000000000000000000, -0.000000000000000000 ) ) ;
#957 = DIRECTION ( 'NONE',  ( 1.000000000000000000, 0.000000000000000000, 0.000000000000000000 ) ) ;
#958 = AXIS2_PLACEMENT_3D ( 'NONE', #3708, #760, #2513 ) ;
#959 = CARTESIAN_POINT ( 'NONE',  ( 0.2073036836782038983, 0.2894590224800283051, -0.0007480297793123734124 ) ) ;
#960 = ORIENTED_EDGE ( 'NONE', *, *, #3981, .F. ) ;
#961 = CYLINDRICAL_SURFACE ( 'NONE', #4264, 0.2362204724409449341 ) ;
#962 = CARTESIAN_POINT ( 'NONE',  ( 0.4685039370078740717, 0.1704774416898499345, 0.2952755905511810774 ) ) ;
#963 = AXIS2_PLACEMENT_3D ( 'NONE', #6501, #1241, #110 ) ;
#964 = ORIENTED_EDGE ( 'NONE', *, *, #3133, .T. ) ;
#965 = ORIENTED_EDGE ( 'NONE', *, *, #7320, .F. ) ;
#966 = DIRECTION ( 'NONE',  ( -1.000000000000000000, -3.491481338843133355E-15, 0.000000000000000000 ) ) ;
#967 = FACE_OUTER_BOUND ( 'NONE', #3872, .T. ) ;
#968 = CARTESIAN_POINT ( 'NONE',  ( 0.4685039370078740717, 0.1704774416898497680, -0.2952755905511810774 ) ) ;
#969 = ORIENTED_EDGE ( 'NONE', *, *, #562, .T. ) ;
#970 = LINE ( 'NONE', #6247, #1429 ) ;
#971 = ORIENTED_EDGE ( 'NONE', *, *, #2285, .T. ) ;
#972 = CARTESIAN_POINT ( 'NONE',  ( 0.8791862816395774605, 0.2121393407445530399, 0.9611380397500175476 ) ) ;
#973 = FILL_AREA_STYLE ('',( #3343 ) ) ;
#974 = ORIENTED_EDGE ( 'NONE', *, *, #1349, .T. ) ;
#975 = AXIS2_PLACEMENT_3D ( 'NONE', #1889, #3025, #4673 ) ;
#976 = DIRECTION ( 'NONE',  ( 0.000000000000000000, 0.000000000000000000, -1.000000000000000000 ) ) ;
#977 = DIRECTION ( 'NONE',  ( 0.000000000000000000, 0.000000000000000000, 1.000000000000000000 ) ) ;
#978 = CARTESIAN_POINT ( 'NONE',  ( 0.9227869198894881331, -0.2286038407206694989, -0.9573410596537438311 ) ) ;
#979 = EDGE_CURVE ( 'NONE', #2951, #5183, #1377, .T. ) ;
#980 = FACE_BOUND ( 'NONE', #696, .T. ) ;
#981 = CARTESIAN_POINT ( 'NONE',  ( 0.4353079511162236126, 0.9479499796399308842, -1.456692913385826849 ) ) ;
#982 = DIRECTION ( 'NONE',  ( 0.000000000000000000, 0.000000000000000000, 1.000000000000000000 ) ) ;
#983 = EDGE_CURVE ( 'NONE', #5247, #1132, #6138, .T. ) ;
#984 = DIRECTION ( 'NONE',  ( -1.000000000000000000, -0.000000000000000000, -4.625929269271482167E-15 ) ) ;
#985 = CARTESIAN_POINT ( 'NONE',  ( 0.9917530546321550178, 0.4509662133831619513, -1.563429817131423372 ) ) ;
#986 = EDGE_CURVE ( 'NONE', #4949, #1484, #5409, .T. ) ;
#987 = ORIENTED_EDGE ( 'NONE', *, *, #3793, .T. ) ;
#988 = CIRCLE ( 'NONE', #5259, 0.2362204724409448231 ) ;
#989 = DIRECTION ( 'NONE',  ( -1.000000000000000000, -0.000000000000000000, -0.000000000000000000 ) ) ;
#990 = ORIENTED_EDGE ( 'NONE', *, *, #5535, .T. ) ;
#991 = CARTESIAN_POINT ( 'NONE',  ( -0.9411660957780404457, 0.4368170150760360415, -1.456692913385826849 ) ) ;
#992 = CARTESIAN_POINT ( 'NONE',  ( 0.3528822938286764188, -0.1453909600788099998, 0.3018098512751525853 ) ) ;
#993 = CIRCLE ( 'NONE', #1973, 0.2362204724409449341 ) ;
#994 = CARTESIAN_POINT ( 'NONE',  ( 0.02637295201093722841, 0.3409548833797004797, 3.882420715168025960E-18 ) ) ;
#995 = ITEM_DEFINED_TRANSFORMATION ( 'NONE', 'NONE', #5772,  #5166 ) ;
#996 = CARTESIAN_POINT ( 'NONE',  ( -0.9479499796399307732, -0.4353079511162269433, -1.456692913385828625 ) ) ;
#997 = VERTEX_POINT ( 'NONE', #6319 ) ;
#998 = CARTESIAN_POINT ( 'NONE',  ( 0.3388536909602617997, 0.2864058322153591463, -0.09448172812127442199 ) ) ;
#999 = CARTESIAN_POINT ( 'NONE',  ( 0.4685039370078740717, 0.000000000000000000, 0.2362204724409449064 ) ) ;
#1000 = VERTEX_POINT ( 'NONE', #2795 ) ;
#1001 = ORIENTED_EDGE ( 'NONE', *, *, #4704, .F. ) ;
#1002 = CARTESIAN_POINT ( 'NONE',  ( 0.000000000000000000, 0.000000000000000000, -0.2952755905511810774 ) ) ;
#1003 = CARTESIAN_POINT ( 'NONE',  ( 0.9921524035015003573, 0.4406690496059847972, -1.439080679658374384 ) ) ;
#1004 = DIRECTION ( 'NONE',  ( 1.000000000000000000, 0.000000000000000000, 0.000000000000000000 ) ) ;
#1005 = VERTEX_POINT ( 'NONE', #616 ) ;
#1006 = DIRECTION ( 'NONE',  ( 0.000000000000000000, 1.000000000000000000, 0.000000000000000000 ) ) ;
#1007 = ORIENTED_EDGE ( 'NONE', *, *, #4073, .F. ) ;
#1008 = LINE ( 'NONE', #2236, #766 ) ;
#1009 = SURFACE_SIDE_STYLE ('',( #6861 ) ) ;
#1010 = ORIENTED_EDGE ( 'NONE', *, *, #5672, .F. ) ;
#1011 = VECTOR ( 'NONE', #271, 39.37007874015748143 ) ;
#1012 = DIMENSIONAL_EXPONENTS ( 1.000000000000000000, 0.000000000000000000, 0.000000000000000000, 0.000000000000000000, 0.000000000000000000, 0.000000000000000000, 0.000000000000000000 ) ;
#1013 = DIRECTION ( 'NONE',  ( -1.000000000000000000, 0.000000000000000000, 0.000000000000000000 ) ) ;
#1014 = DIRECTION ( 'NONE',  ( -1.000000000000000000, 1.224646799147353700E-16, 0.000000000000000000 ) ) ;
#1015 = LINE ( 'NONE', #1730, #5372 ) ;
#1016 = TOROIDAL_SURFACE ( 'NONE', #5285, 1.043121362164705745, 0.05905511811023622659 ) ;
#1017 = DIRECTION ( 'NONE',  ( 0.000000000000000000, 1.000000000000000000, 0.000000000000000000 ) ) ;
#1018 = EDGE_CURVE ( 'NONE', #5096, #997, #4629, .T. ) ;
#1019 = CARTESIAN_POINT ( 'NONE',  ( 0.9159926810392130525, -0.4466264210910701471, -1.451746030331783510 ) ) ;
#1020 = CARTESIAN_POINT ( 'NONE',  ( 0.4330708661417324024, 5.520553484345353405E-17, -0.4507874015748032370 ) ) ;
#1021 = CARTESIAN_POINT ( 'NONE',  ( 0.3321022367507227568, -0.2411754471855062087, 0.1728230530389214537 ) ) ;
#1022 = CARTESIAN_POINT ( 'NONE',  ( 0.02637295201093722841, 0.3409548833797004797, 3.882420715168025960E-18 ) ) ;
#1023 = DIRECTION ( 'NONE',  ( -0.000000000000000000, -0.000000000000000000, 1.000000000000000000 ) ) ;
#1024 = DIRECTION ( 'NONE',  ( 1.000000000000000000, 0.000000000000000000, 0.000000000000000000 ) ) ;
#1025 = AXIS2_PLACEMENT_3D ( 'NONE', #5708, #3980, #2817 ) ;
#1026 = ORIENTED_EDGE ( 'NONE', *, *, #5761, .T. ) ;
#1027 = CARTESIAN_POINT ( 'NONE',  ( 0.3336175750056032951, 0.05682581389661665178, 0.2952755905511811885 ) ) ;
#1028 = EDGE_CURVE ( 'NONE', #6588, #4456, #3758, .T. ) ;
#1029 = EDGE_CURVE ( 'NONE', #4985, #3143, #5268, .T. ) ;
#1030 = CARTESIAN_POINT ( 'NONE',  ( 0.3997746709170348356, 0.000000000000000000, 0.000000000000000000 ) ) ;
#1031 = B_SPLINE_CURVE_WITH_KNOTS ( 'NONE', 3,
 ( #2435, #718, #5924, #605, #6410, #4115, #3621, #7100, #5266, #3543 ),
 .UNSPECIFIED., .F., .F.,
 ( 4, 2, 2, 2, 4 ),
 ( -7.765797721852544519E-06, 0.0005114169989440498724, 0.001030599795609952150, 0.001549782592275854428, 0.002068965388941757140 ),
 .UNSPECIFIED. ) ;
#1032 = CIRCLE ( 'NONE', #7255, 0.9964144355006141485 ) ;
#1033 = EDGE_CURVE ( 'NONE', #4777, #2217, #729, .T. ) ;
#1034 = CARTESIAN_POINT ( 'NONE',  ( 0.3306743754077736130, -0.2557161625347756373, -0.1476377952755904555 ) ) ;
#1035 = EDGE_LOOP ( 'NONE', ( #1136, #3060, #3296, #41, #3711 ) ) ;
#1036 = CARTESIAN_POINT ( 'NONE',  ( 0.002513486811083733702, -0.2268523693227597338, -0.1976313516179637741 ) ) ;
#1037 = CARTESIAN_POINT ( 'NONE',  ( 0.3531511627980793433, -0.1878266560944103492, 0.2783075040405565415 ) ) ;
#1038 = ORIENTED_EDGE ( 'NONE', *, *, #6836, .T. ) ;
#1039 = EDGE_LOOP ( 'NONE', ( #649, #2721, #2871, #3146 ) ) ;
#1040 = ADVANCED_FACE ( 'NONE', ( #6510, #6546, #3016 ), #1878, .F. ) ;
#1041 = CARTESIAN_POINT ( 'NONE',  ( 0.9998202959290236613, -0.2362140621487221481, 0.9554867107345892396 ) ) ;
#1042 = CARTESIAN_POINT ( 'NONE',  ( 0.3483227611829846082, 0.1704774416898497680, -0.2952755905511810774 ) ) ;
#1043 = ORIENTED_EDGE ( 'NONE', *, *, #3, .F. ) ;
#1044 = CARTESIAN_POINT ( 'NONE',  ( 0.3483227611829846637, 0.1704774416898499345, 0.2952755905511810774 ) ) ;
#1045 = VERTEX_POINT ( 'NONE', #4169 ) ;
#1046 = DIRECTION ( 'NONE',  ( 4.647695938698652561E-15, 0.000000000000000000, -1.000000000000000000 ) ) ;
#1047 = EDGE_LOOP ( 'NONE', ( #1242, #1268, #6541, #3497 ) ) ;
#1048 = CARTESIAN_POINT ( 'NONE',  ( 0.000000000000000000, 0.000000000000000000, 0.1188976377952756375 ) ) ;
#1049 = DIRECTION ( 'NONE',  ( -5.157119279425400316E-32, -1.000000000000000000, 1.795077641733698726E-27 ) ) ;
#1050 = CARTESIAN_POINT ( 'NONE',  ( 0.8833361873720787516, 0.4663632139997673232, -1.436953241411981663 ) ) ;
#1051 = DIRECTION ( 'NONE',  ( 0.000000000000000000, 0.000000000000000000, 1.000000000000000000 ) ) ;
#1052 = DIRECTION ( 'NONE',  ( -1.224646799147353207E-16, -1.000000000000000000, -0.000000000000000000 ) ) ;
#1053 = CARTESIAN_POINT ( 'NONE',  ( 0.8403423717953923955, 0.1874820019069840249, -0.9662438517680175254 ) ) ;
#1054 = CARTESIAN_POINT ( 'NONE',  ( -0.5072022184711438841, -1.064268091467010846, -1.491294347567248435 ) ) ;
#1055 = CARTESIAN_POINT ( 'NONE',  ( -0.3543307086614173040, 0.06965032677943189254, -0.003053646640237103489 ) ) ;
#1056 = CARTESIAN_POINT ( 'NONE',  ( 3.198568410424924124, 2.407012729153881203, 2.480314960629921295 ) ) ;
#1057 = CARTESIAN_POINT ( 'NONE',  ( -0.2066929133858267931, 2.531258147843938473E-17, -0.4082677165354330340 ) ) ;
#1058 = PRODUCT_RELATED_PRODUCT_CATEGORY ( 'part', '', ( #141 ) ) ;
#1059 = CARTESIAN_POINT ( 'NONE',  ( 0.3391892065151629887, 0.1136516277932332897, 0.2952755905511810774 ) ) ;
#1060 = CARTESIAN_POINT ( 'NONE',  ( 0.3496875133419357629, -0.1780312604149854316, -0.2952755905511810774 ) ) ;
#1061 = CIRCLE ( 'NONE', #5339, 0.2066929133858267931 ) ;
#1062 = CARTESIAN_POINT ( 'NONE',  ( 0.3254211578371890567, 0.2212638669783392742, -0.02201102547170719764 ) ) ;
#1063 = FACE_OUTER_BOUND ( 'NONE', #3751, .T. ) ;
#1064 = ORIENTED_EDGE ( 'NONE', *, *, #2383, .F. ) ;
#1065 = CARTESIAN_POINT ( 'NONE',  ( 0.3442723180357227797, 0.1814473180894613513, -0.2762752072743030474 ) ) ;
#1066 = CARTESIAN_POINT ( 'NONE',  ( 0.1771653543307089296, 0.3068593950417301541, -0.4082677165354330340 ) ) ;
#1067 = ADVANCED_FACE ( 'NONE', ( #7072 ), #656, .F. ) ;
#1068 = VERTEX_POINT ( 'NONE', #1784 ) ;
#1069 = CIRCLE ( 'NONE', #2782, 0.2952755905511810774 ) ;
#1070 = ORIENTED_EDGE ( 'NONE', *, *, #6917, .T. ) ;
#1071 = CARTESIAN_POINT ( 'NONE',  ( 1.162092266633492077, -0.1562322077656922159, 0.9718357064180906946 ) ) ;
#1072 = ORIENTED_EDGE ( 'NONE', *, *, #4997, .T. ) ;
#1073 = CARTESIAN_POINT ( 'NONE',  ( -1.861696953619914682E-15, 0.000000000000000000, -1.361499588670820771 ) ) ;
#1074 = VERTEX_POINT ( 'NONE', #2977 ) ;
#1075 = CIRCLE ( 'NONE', #7179, 1.089828288828796676 ) ;
#1076 = DIRECTION ( 'NONE',  ( 0.000000000000000000, 0.000000000000000000, -1.000000000000000000 ) ) ;
#1077 = EDGE_CURVE ( 'NONE', #2114, #4878, #5583, .T. ) ;
#1078 = EDGE_CURVE ( 'NONE', #139, #7188, #6372, .T. ) ;
#1079 = VERTEX_POINT ( 'NONE', #3135 ) ;
#1080 = ORIENTED_EDGE ( 'NONE', *, *, #6315, .F. ) ;
#1081 = EDGE_CURVE ( 'NONE', #3879, #1683, #94, .T. ) ;
#1082 = DIRECTION ( 'NONE',  ( -1.000000000000000000, 0.000000000000000000, 0.000000000000000000 ) ) ;
#1083 = CIRCLE ( 'NONE', #3902, 0.2362204724409448231 ) ;
#1084 = DIRECTION ( 'NONE',  ( -2.320548612096681119E-16, 8.648785545355717899E-18, 1.000000000000000000 ) ) ;
#1085 = CARTESIAN_POINT ( 'NONE',  ( 0.3581828924050327045, -0.3486337532542230222, -1.123169198254405176E-18 ) ) ;
#1086 = DIRECTION ( 'NONE',  ( 1.000000000000000000, 0.000000000000000000, -0.000000000000000000 ) ) ;
#1087 = CONICAL_SURFACE ( 'NONE', #1815, 0.3543307086614173596, 1.047197551196596521 ) ;
#1088 = LINE ( 'NONE', #5499, #1099 ) ;
#1089 = AXIS2_PLACEMENT_3D ( 'NONE', #3426, #2167, #413 ) ;
#1090 = DIRECTION ( 'NONE',  ( 1.000000000000000000, 0.000000000000000000, 0.000000000000000000 ) ) ;
#1091 = CARTESIAN_POINT ( 'NONE',  ( -1.781909941321919274E-15, 0.000000000000000000, -1.397637795275591843 ) ) ;
#1092 = CARTESIAN_POINT ( 'NONE',  ( 3.414809992080329023E-17, 0.4091458600556405201, -0.03164754241312491001 ) ) ;
#1093 = CARTESIAN_POINT ( 'NONE',  ( 0.000000000000000000, 0.000000000000000000, -0.7983802283864780414 ) ) ;
#1094 = DIRECTION ( 'NONE',  ( 1.000000000000000000, 0.000000000000000000, -0.000000000000000000 ) ) ;
#1095 = ORIENTED_EDGE ( 'NONE', *, *, #6551, .T. ) ;
#1096 = CARTESIAN_POINT ( 'NONE',  ( 0.000000000000000000, 0.000000000000000000, 0.000000000000000000 ) ) ;
#1097 = FACE_BOUND ( 'NONE', #2604, .T. ) ;
#1098 = ORIENTED_EDGE ( 'NONE', *, *, #4460, .F. ) ;
#1099 = VECTOR ( 'NONE', #5457, 39.37007874015748143 ) ;
#1100 = ORIENTED_EDGE ( 'NONE', *, *, #3555, .T. ) ;
#1101 = DIRECTION ( 'NONE',  ( -1.000000000000000000, 0.000000000000000000, 0.000000000000000000 ) ) ;
#1102 = CARTESIAN_POINT ( 'NONE',  ( 0.3391892065151629332, 0.1136516277932330399, -0.2952755905511810774 ) ) ;
#1103 = CARTESIAN_POINT ( 'NONE',  ( 0.3527008206095850751, 0.1709223649093223329, 0.2960462201727743214 ) ) ;
#1104 = ORIENTED_EDGE ( 'NONE', *, *, #7014, .F. ) ;
#1105 = AXIS2_PLACEMENT_3D ( 'NONE', #805, #957, #881 ) ;
#1106 = CARTESIAN_POINT ( 'NONE',  ( 0.02637295201093703412, 0.1704774416898499345, 0.2952755905511810774 ) ) ;
#1107 = FACE_OUTER_BOUND ( 'NONE', #2197, .T. ) ;
#1108 = VERTEX_POINT ( 'NONE', #3632 ) ;
#1109 = CARTESIAN_POINT ( 'NONE',  ( 0.3543307086614173040, 0.2045729300278199825, -0.4082677165354330340 ) ) ;
#1110 = ADVANCED_FACE ( 'NONE', ( #1952 ), #5444, .F. ) ;
#1111 = ADVANCED_FACE ( 'NONE', ( #4245 ), #396, .T. ) ;
#1112 = PRODUCT_CONTEXT ( 'NONE', #7449, 'mechanical' ) ;
#1113 = CONICAL_SURFACE ( 'NONE', #3691, 0.3543307086614173596, 1.047197551196596521 ) ;
#1114 = PLANE ( 'NONE',  #1089 ) ;
#1115 = EDGE_CURVE ( 'NONE', #4304, #4703, #3678, .T. ) ;
#1116 = AXIS2_PLACEMENT_3D ( 'NONE', #678, #3002, #5337 ) ;
#1117 = FACE_OUTER_BOUND ( 'NONE', #3223, .T. ) ;
#1118 = CARTESIAN_POINT ( 'NONE',  ( -0.3543307086614173040, 0.2045729300278199547, -0.03164754241312472960 ) ) ;
#1119 = EDGE_CURVE ( 'NONE', #358, #1383, #7289, .T. ) ;
#1120 = AXIS2_PLACEMENT_3D ( 'NONE', #5408, #3520, #581 ) ;
#1121 = DIRECTION ( 'NONE',  ( -0.000000000000000000, -0.000000000000000000, -1.000000000000000000 ) ) ;
#1122 = CARTESIAN_POINT ( 'NONE',  ( 21.65354330708661479, 0.000000000000000000, 0.000000000000000000 ) ) ;
#1123 = CARTESIAN_POINT ( 'NONE',  ( 0.3479975484506714345, 0.1192183696110101915, -0.3017044215715822819 ) ) ;
#1124 = LINE ( 'NONE', #6236, #3590 ) ;
#1125 = FACE_OUTER_BOUND ( 'NONE', #800, .T. ) ;
#1126 = CARTESIAN_POINT ( 'NONE',  ( 0.4685039370078740717, -0.3409548833797009237, 0.000000000000000000 ) ) ;
#1127 = ORIENTED_EDGE ( 'NONE', *, *, #1920, .F. ) ;
#1128 = DIRECTION ( 'NONE',  ( -0.000000000000000000, -0.000000000000000000, -1.000000000000000000 ) ) ;
#1129 = DIRECTION ( 'NONE',  ( 0.000000000000000000, 0.000000000000000000, -1.000000000000000000 ) ) ;
#1130 = CARTESIAN_POINT ( 'NONE',  ( 0.3403864257300880936, 0.2851194846584802489, 0.09670974744601845696 ) ) ;
#1131 = ORIENTED_EDGE ( 'NONE', *, *, #5382, .T. ) ;
#1132 = VERTEX_POINT ( 'NONE', #5343 ) ;
#1133 = AXIS2_PLACEMENT_3D ( 'NONE', #6885, #7481, #2747 ) ;
#1134 = CARTESIAN_POINT ( 'NONE',  ( 1.128523761465410891, -0.1876879802734073011, 0.9662312300142489319 ) ) ;
#1135 = CARTESIAN_POINT ( 'NONE',  ( 0.4685039370078740717, 5.594759879304195485E-17, -0.4507874015748032370 ) ) ;
#1136 = ORIENTED_EDGE ( 'NONE', *, *, #4590, .T. ) ;
#1137 = CARTESIAN_POINT ( 'NONE',  ( -0.2371803407075529779, -0.2722097265016479306, -0.4046248963849241043 ) ) ;
#1138 = CARTESIAN_POINT ( 'NONE',  ( 0.000000000000000000, 0.000000000000000000, 0.000000000000000000 ) ) ;
#1139 = DIRECTION ( 'NONE',  ( -1.000000000000000000, -0.000000000000000000, -0.000000000000000000 ) ) ;
#1140 = VERTEX_POINT ( 'NONE', #2478 ) ;
#1141 = CYLINDRICAL_SURFACE ( 'NONE', #2110, 0.2362204724409449064 ) ;
#1142 = DIRECTION ( 'NONE',  ( 0.000000000000000000, 0.000000000000000000, 1.000000000000000000 ) ) ;
#1143 = CARTESIAN_POINT ( 'NONE',  ( 7.874015748031496287, 0.000000000000000000, -0.2362204724409455170 ) ) ;
#1144 = CARTESIAN_POINT ( 'NONE',  ( 3.414809992080329023E-17, 0.4091458600556405201, -0.3766201741223081378 ) ) ;
#1145 = CARTESIAN_POINT ( 'NONE',  ( 0.4685039370078740717, 0.3409548833797004797, 2.164902785881980513E-17 ) ) ;
#1146 = EDGE_CURVE ( 'NONE', #735, #5146, #6301, .T. ) ;
#1147 = EDGE_CURVE ( 'NONE', #3264, #3796, #6256, .T. ) ;
#1148 = ORIENTED_EDGE ( 'NONE', *, *, #1028, .T. ) ;
#1149 = ADVANCED_FACE ( 'NONE', ( #596 ), #6529, .T. ) ;
#1150 = CARTESIAN_POINT ( 'NONE',  ( 3.198568410424924124, 2.407012729153881203, 0.4724409448818898127 ) ) ;
#1151 = DIRECTION ( 'NONE',  ( 0.000000000000000000, 0.000000000000000000, -1.000000000000000000 ) ) ;
#1152 = DIRECTION ( 'NONE',  ( 0.000000000000000000, 0.000000000000000000, -1.000000000000000000 ) ) ;
#1153 = EDGE_CURVE ( 'NONE', #1896, #3901, #1935, .T. ) ;
#1154 = EDGE_CURVE ( 'NONE', #6581, #34, #5730, .T. ) ;
#1155 = AXIS2_PLACEMENT_3D ( 'NONE', #6972, #1795, #7082 ) ;
#1156 = CARTESIAN_POINT ( 'NONE',  ( -0.4700904924197903401, -0.9659644734970543878, -1.546597720061111847 ) ) ;
#1157 = CARTESIAN_POINT ( 'NONE',  ( -0.4377665650305635481, 0.9883301303667336724, -1.443420399700355850 ) ) ;
#1158 = CARTESIAN_POINT ( 'NONE',  ( 0.3483227611829846637, 0.1704774416898499345, 0.2952755905511810774 ) ) ;
#1159 = CARTESIAN_POINT ( 'NONE',  ( 0.000000000000000000, 0.000000000000000000, -0.4082677165354330340 ) ) ;
#1160 = CARTESIAN_POINT ( 'NONE',  ( 0.3410249605999410294, 1.062103031354818709E-12, 0.3014927230551906479 ) ) ;
#1161 = ORIENTED_EDGE ( 'NONE', *, *, #99, .T. ) ;
#1162 = FACE_BOUND ( 'NONE', #629, .T. ) ;
#1163 = DIRECTION ( 'NONE',  ( 0.000000000000000000, 0.000000000000000000, 1.000000000000000000 ) ) ;
#1164 = ORIENTED_EDGE ( 'NONE', *, *, #4822, .T. ) ;
#1165 = ORIENTED_EDGE ( 'NONE', *, *, #5580, .F. ) ;
#1166 = DIRECTION ( 'NONE',  ( -1.000000000000000000, 0.000000000000000000, 0.000000000000000000 ) ) ;
#1167 = CIRCLE ( 'NONE', #4113, 1.278433327952056553 ) ;
#1168 = CARTESIAN_POINT ( 'NONE',  ( 0.7480314960629922405, 1.220472440944881942, 2.480314960629921295 ) ) ;
#1169 = B_SPLINE_CURVE_WITH_KNOTS ( 'NONE', 3,
 ( #1939, #6254, #3965, #2128, #6863, #7207 ),
 .UNSPECIFIED., .F., .F.,
 ( 4, 2, 4 ),
 ( 0.000000000000000000, 0.002233368740102889029, 0.004466737480205778058 ),
 .UNSPECIFIED. ) ;
#1170 = VERTEX_POINT ( 'NONE', #6973 ) ;
#1171 = AXIS2_PLACEMENT_3D ( 'NONE', #3053, #2405, #4741 ) ;
#1172 = CARTESIAN_POINT ( 'NONE',  ( 0.9842519685039370358, 0.7480314960629921295, 0.000000000000000000 ) ) ;
#1173 = B_SPLINE_CURVE_WITH_KNOTS ( 'NONE', 3,
 ( #235, #3207, #6691, #5477, #2555, #1434 ),
 .UNSPECIFIED., .F., .F.,
 ( 4, 2, 4 ),
 ( 2.380730968201871590E-07, 0.002629065763328350055, 0.005257893453559879353 ),
 .UNSPECIFIED. ) ;
#1174 = ORIENTED_EDGE ( 'NONE', *, *, #3375, .T. ) ;
#1175 = DIRECTION ( 'NONE',  ( 1.000000000000000000, 0.000000000000000000, 0.000000000000000000 ) ) ;
#1176 = CARTESIAN_POINT ( 'NONE',  ( 0.3403859949404050012, 0.05880135802647309951, 0.2952755905511811330 ) ) ;
#1177 = VECTOR ( 'NONE', #5049, 39.37007874015748143 ) ;
#1178 = DIRECTION ( 'NONE',  ( 0.000000000000000000, 0.000000000000000000, -1.000000000000000000 ) ) ;
#1179 = ORIENTED_EDGE ( 'NONE', *, *, #4704, .T. ) ;
#1180 = CARTESIAN_POINT ( 'NONE',  ( -0.4437903857718329403, -0.9221073153504530939, -1.453484209829405849 ) ) ;
#1181 = ORIENTED_EDGE ( 'NONE', *, *, #5950, .T. ) ;
#1182 = CARTESIAN_POINT ( 'NONE',  ( 0.3306743754077735575, 0.2557161625347751932, -0.1476377952755904832 ) ) ;
#1183 =( REPRESENTATION_RELATIONSHIP ('NONE','NONE', #303, #2912 ) REPRESENTATION_RELATIONSHIP_WITH_TRANSFORMATION ( #1477 )SHAPE_REPRESENTATION_RELATIONSHIP( ) );
#1184 = CIRCLE ( 'NONE', #963, 0.2362204724409448231 ) ;
#1185 = ORIENTED_EDGE ( 'NONE', *, *, #427, .T. ) ;
#1186 = B_SPLINE_CURVE_WITH_KNOTS ( 'NONE', 3,
 ( #818, #2645, #3258, #7268, #4908, #6740, #4372, #325, #1491, #3842, #3764, #1382, #6066, #6173, #6706, #1451, #6672, #252 ),
 .UNSPECIFIED., .F., .F.,
 ( 4, 2, 2, 2, 2, 2, 2, 2, 4 ),
 ( -8.121667112575779769E-06, 0.0009422843086939633418, 0.001417487296597240952, 0.001892690284500518237, 0.002367893272403795522, 0.002843096260307073023, 0.003318299248210350091, 0.003555900742161984072, 0.003793502236113618052 ),
 .UNSPECIFIED. ) ;
#1187 = SHAPE_REPRESENTATION_RELATIONSHIP ( 'NONE' , 'NONE' ,  #2104, #2576 ) ;
#1188 = B_SPLINE_CURVE_WITH_KNOTS ( 'NONE', 3,
 ( #4271, #6609, #1358, #5082, #5120, #3854 ),
 .UNSPECIFIED., .F., .F.,
 ( 4, 2, 4 ),
 ( 2.380730968228139670E-07, 0.002629065763328361331, 0.005257893453559899302 ),
 .UNSPECIFIED. ) ;
#1189 = ADVANCED_FACE ( 'NONE', ( #6547 ), #3490, .T. ) ;
#1190 = CARTESIAN_POINT ( 'NONE',  ( 3.198568410424924124, 2.407012729153881203, 2.480314960629921295 ) ) ;
#1191 = DIRECTION ( 'NONE',  ( 0.000000000000000000, 0.000000000000000000, -1.000000000000000000 ) ) ;
#1192 = TOROIDAL_SURFACE ( 'NONE', #2547, 1.124634398195722973, 0.05905511811023622659 ) ;
#1193 = DIRECTION ( 'NONE',  ( -1.000000000000000000, -1.776356839400250465E-15, 0.000000000000000000 ) ) ;
#1194 = CARTESIAN_POINT ( 'NONE',  ( 0.3442725010713152956, -0.1485386763991280168, -0.2952755905511810774 ) ) ;
#1195 = AXIS2_PLACEMENT_3D ( 'NONE', #1895, #3110, #7240 ) ;
#1196 = CARTESIAN_POINT ( 'NONE',  ( -0.4353079511162236681, -0.9479499796399322165, -1.456692913385828625 ) ) ;
#1197 = CARTESIAN_POINT ( 'NONE',  ( 1.968503937007874072, 1.496062992125984259, 0.000000000000000000 ) ) ;
#1198 = CARTESIAN_POINT ( 'NONE',  ( -2.834645669291338432, 0.000000000000000000, 0.4724409448818898127 ) ) ;
#1199 = EDGE_CURVE ( 'NONE', #5611, #1, #5894, .T. ) ;
#1200 = EDGE_CURVE ( 'NONE', #709, #5935, #5666, .T. ) ;
#1201 = CARTESIAN_POINT ( 'NONE',  ( 21.65354330708661479, 0.000000000000000000, 0.000000000000000000 ) ) ;
#1202 = DIRECTION ( 'NONE',  ( 0.000000000000000000, -0.000000000000000000, 1.000000000000000000 ) ) ;
#1203 = ORIENTED_EDGE ( 'NONE', *, *, #3271, .T. ) ;
#1204 = AXIS2_PLACEMENT_3D ( 'NONE', #454, #2271, #2874 ) ;
#1205 = CARTESIAN_POINT ( 'NONE',  ( 1.968503937007874072, 1.496062992125984259, -0.2362204724409449619 ) ) ;
#1206 = DIRECTION ( 'NONE',  ( -0.000000000000000000, -0.000000000000000000, 1.000000000000000000 ) ) ;
#1207 = ORIENTED_EDGE ( 'NONE', *, *, #7509, .F. ) ;
#1208 = VERTEX_POINT ( 'NONE', #3203 ) ;
#1209 = CARTESIAN_POINT ( 'NONE',  ( 0.7480314960629923515, 1.544184662414706467E-22, 0.9842519685039370358 ) ) ;
#1210 = LINE ( 'NONE', #5977, #223 ) ;
#1211 = EDGE_LOOP ( 'NONE', ( #3226, #6021, #4866, #3846 ) ) ;
#1212 = FACE_OUTER_BOUND ( 'NONE', #6387, .T. ) ;
#1213 = TOROIDAL_SURFACE ( 'NONE', #4042, 1.223643328182682621, 0.05905511811023622659 ) ;
#1214 = CARTESIAN_POINT ( 'NONE',  ( -0.5118110236220474452, 1.220472440944881942, 0.000000000000000000 ) ) ;
#1215 = ORIENTED_EDGE ( 'NONE', *, *, #2294, .T. ) ;
#1216 = PRODUCT ( 'Base', 'Base', '', ( #5055 ) ) ;
#1217 = DIRECTION ( 'NONE',  ( 1.000000000000000000, 0.000000000000000000, 0.000000000000000000 ) ) ;
#1218 = CARTESIAN_POINT ( 'NONE',  ( 0.3442721343065135997, 0.1485366976410457951, 0.2952755905511810774 ) ) ;
#1219 = DIRECTION ( 'NONE',  ( -1.000000000000000000, 0.000000000000000000, 0.000000000000000000 ) ) ;
#1220 = AXIS2_PLACEMENT_3D ( 'NONE', #4895, #5015, #2070 ) ;
#1221 = LINE ( 'NONE', #5368, #2900 ) ;
#1222 = CARTESIAN_POINT ( 'NONE',  ( -1.054581703806070525, -0.4332776154273933478, -1.572814851683855597 ) ) ;
#1223 = VECTOR ( 'NONE', #2809, 39.37007874015748143 ) ;
#1224 = ORIENTED_EDGE ( 'NONE', *, *, #2013, .T. ) ;
#1225 = DIRECTION ( 'NONE',  ( -1.000000000000000000, 0.000000000000000000, -2.193342766891360832E-15 ) ) ;
#1226 = CARTESIAN_POINT ( 'NONE',  ( -0.4333661275892026765, 1.041228047528455658, -1.574803149606299302 ) ) ;
#1227 = ORIENTED_EDGE ( 'NONE', *, *, #7241, .T. ) ;
#1228 = AXIS2_PLACEMENT_3D ( 'NONE', #4210, #3052, #7030 ) ;
#1229 = CARTESIAN_POINT ( 'NONE',  ( 0.9479499796399352141, -0.4353079511162137316, -1.456692913385826849 ) ) ;
#1230 = DIRECTION ( 'NONE',  ( -1.000000000000000000, 0.000000000000000000, 0.000000000000000000 ) ) ;
#1231 = SURFACE_STYLE_USAGE ( .BOTH. , #184 ) ;
#1232 = AXIS2_PLACEMENT_3D ( 'NONE', #3485, #1076, #6420 ) ;
#1233 = DIRECTION ( 'NONE',  ( -1.000000000000000000, 0.000000000000000000, 0.000000000000000000 ) ) ;
#1234 = CIRCLE ( 'NONE', #6630, 0.2362204724409449896 ) ;
#1235 = CARTESIAN_POINT ( 'NONE',  ( -0.9541934910893046240, 0.4339190921229418296, -1.456692913385826849 ) ) ;
#1236 = CARTESIAN_POINT ( 'NONE',  ( 0.3543307086614172485, 0.000000000000000000, 7.886165872636028972E-17 ) ) ;
#1237 = CARTESIAN_POINT ( 'NONE',  ( -0.4700904924197871204, 0.000000000000000000, -2.204724409448822975 ) ) ;
#1238 = DIRECTION ( 'NONE',  ( -1.000000000000000000, -0.000000000000000000, -0.000000000000000000 ) ) ;
#1239 = CARTESIAN_POINT ( 'NONE',  ( 0.3426022948973417859, 0.05819196463765207578, 0.3015401604570892014 ) ) ;
#1240 = DIRECTION ( 'NONE',  ( -0.000000000000000000, -0.000000000000000000, 1.000000000000000000 ) ) ;
#1241 = DIRECTION ( 'NONE',  ( -0.000000000000000000, -0.000000000000000000, 1.000000000000000000 ) ) ;
#1242 = ORIENTED_EDGE ( 'NONE', *, *, #946, .F. ) ;
#1243 = AXIS2_PLACEMENT_3D ( 'NONE', #5009, #4546, #7326 ) ;
#1244 = PLANE ( 'NONE',  #3948 ) ;
#1245 = CARTESIAN_POINT ( 'NONE',  ( 0.3581828924050323715, -0.1743168766271109560, 0.3019256869348722616 ) ) ;
#1246 = EDGE_CURVE ( 'NONE', #3477, #1972, #5940, .T. ) ;
#1247 = EDGE_CURVE ( 'NONE', #6856, #1132, #5587, .T. ) ;
#1248 = VERTEX_POINT ( 'NONE', #948 ) ;
#1249 = ORIENTED_EDGE ( 'NONE', *, *, #2569, .T. ) ;
#1250 = CARTESIAN_POINT ( 'NONE',  ( 0.1621299108466741079, -0.3155401123846236500, -3.166369226054953705E-17 ) ) ;
#1251 = EDGE_CURVE ( 'NONE', #5818, #4818, #869, .T. ) ;
#1252 = CYLINDRICAL_SURFACE ( 'NONE', #5601, 1.968503937007874072 ) ;
#1253 = EDGE_LOOP ( 'NONE', ( #516, #1922 ) ) ;
#1254 = CARTESIAN_POINT ( 'NONE',  ( 0.3528999085283636150, -0.1454870853231272354, -0.3018102362147644380 ) ) ;
#1255 = B_SPLINE_CURVE_WITH_KNOTS ( 'NONE', 3,
 ( #2340, #4984, #1490, #4948, #6101, #3797, #7192, #6135 ),
 .UNSPECIFIED., .F., .F.,
 ( 4, 2, 2, 4 ),
 ( 0.004381617662950723809, 0.005472867551409551883, 0.006564117439868379089, 0.008746617216786035237 ),
 .UNSPECIFIED. ) ;
#1256 = FACE_OUTER_BOUND ( 'NONE', #7123, .T. ) ;
#1257 = EDGE_CURVE ( 'NONE', #2327, #5278, #5181, .T. ) ;
#1258 = VERTEX_POINT ( 'NONE', #3819 ) ;
#1259 = VECTOR ( 'NONE', #5923, 39.37007874015748143 ) ;
#1260 = MECHANICAL_DESIGN_GEOMETRIC_PRESENTATION_REPRESENTATION (  '', ( #5795 ), #4688 ) ;
#1261 = VERTEX_POINT ( 'NONE', #7322 ) ;
#1262 = CARTESIAN_POINT ( 'NONE',  ( 0.000000000000000000, 0.000000000000000000, 0.3732633159281743551 ) ) ;
#1263 = CARTESIAN_POINT ( 'NONE',  ( 0.3426140154788509529, 0.05854580700589206294, 0.3015405874046677703 ) ) ;
#1264 = CONTEXT_DEPENDENT_SHAPE_REPRESENTATION ( #6151, #7276 ) ;
#1265 = LENGTH_MEASURE_WITH_UNIT ( LENGTH_MEASURE( 0.02539999999999999897 ), #1301 );
#1266 = LINE ( 'NONE', #5952, #4999 ) ;
#1267 = ORIENTED_EDGE ( 'NONE', *, *, #1876, .F. ) ;
#1268 = ORIENTED_EDGE ( 'NONE', *, *, #5904, .T. ) ;
#1269 = CARTESIAN_POINT ( 'NONE',  ( 0.3321022367506965556, -0.2702568778840481745, -0.1224525375122541698 ) ) ;
#1270 = CYLINDRICAL_SURFACE ( 'NONE', #6715, 0.2699662542182227343 ) ;
#1271 =( CONVERSION_BASED_UNIT ( 'INCH', #1351 ) LENGTH_UNIT ( ) NAMED_UNIT ( #5074 ) );
#1272 = B_SPLINE_CURVE_WITH_KNOTS ( 'NONE', 3,
 ( #1156, #1862, #2352, #1317, #6534, #3620, #5962, #3042 ),
 .UNSPECIFIED., .F., .F.,
 ( 4, 2, 2, 4 ),
 ( -7.690028535482676563E-06, 0.001102852776893268553, 0.001658124179607648385, 0.002213395582322028217 ),
 .UNSPECIFIED. ) ;
#1273 = DIRECTION ( 'NONE',  ( 1.000000000000000000, 0.000000000000000000, 0.000000000000000000 ) ) ;
#1274 = PRODUCT_DEFINITION_CONTEXT ( 'detailed design', #438, 'design' ) ;
#1275 = CARTESIAN_POINT ( 'NONE',  ( 0.4882975260543730434, -0.9867938558989103326, -1.385219839936550956 ) ) ;
#1276 = CARTESIAN_POINT ( 'NONE',  ( 0.000000000000000000, 0.000000000000000000, -0.4921259842519685179 ) ) ;
#1277 = DIRECTION ( 'NONE',  ( -0.000000000000000000, 0.000000000000000000, 1.000000000000000000 ) ) ;
#1278 = DIRECTION ( 'NONE',  ( 1.000000000000000000, 0.000000000000000000, 0.000000000000000000 ) ) ;
#1279 = CARTESIAN_POINT ( 'NONE',  ( 0.3336175750056034617, -0.2841290694830840846, -0.09842519685039370636 ) ) ;
#1280 = DIRECTION ( 'NONE',  ( -0.000000000000000000, 0.8660254037844383745, 0.5000000000000006661 ) ) ;
#1281 = LINE ( 'NONE', #1908, #5738 ) ;
#1282 = EDGE_LOOP ( 'NONE', ( #4826, #6098, #395 ) ) ;
#1283 = PRODUCT_DEFINITION_SHAPE ( 'NONE', 'NONE',  #3831 ) ;
#1284 = DIRECTION ( 'NONE',  ( 0.000000000000000000, 0.000000000000000000, -1.000000000000000000 ) ) ;
#1285 = CARTESIAN_POINT ( 'NONE',  ( 0.3485373078438442351, -0.2031105961982146157, 0.2516016230262508313 ) ) ;
#1286 = AXIS2_PLACEMENT_3D ( 'NONE', #6181, #4572, #1084 ) ;
#1287 = ORIENTED_EDGE ( 'NONE', *, *, #1336, .T. ) ;
#1288 = CARTESIAN_POINT ( 'NONE',  ( 0.7719899816204534027, -0.1048018568659492278, 0.9787612993317383880 ) ) ;
#1289 = APPLICATION_CONTEXT ( 'automotive_design' ) ;
#1290 = EDGE_CURVE ( 'NONE', #2401, #2222, #3676, .T. ) ;
#1291 = DIRECTION ( 'NONE',  ( 1.000000000000000000, 0.000000000000000000, 0.000000000000000000 ) ) ;
#1292 = FACE_OUTER_BOUND ( 'NONE', #5354, .T. ) ;
#1293 = EDGE_LOOP ( 'NONE', ( #1989, #3770, #5608, #4332 ) ) ;
#1294 = CARTESIAN_POINT ( 'NONE',  ( -0.3543307086614173040, -0.1372236123666514540, -0.01398679180475823590 ) ) ;
#1295 = ORIENTED_EDGE ( 'NONE', *, *, #5577, .T. ) ;
#1296 = VERTEX_POINT ( 'NONE', #5627 ) ;
#1297 = CARTESIAN_POINT ( 'NONE',  ( 0.3585665126877357611, -0.3496831043983833487, 0.001800812819183493984 ) ) ;
#1298 = CARTESIAN_POINT ( 'NONE',  ( 0.3496779098333545610, -0.1779789496721726760, 0.2952755905511811330 ) ) ;
#1299 = SHAPE_DEFINITION_REPRESENTATION ( #1469, #7075 ) ;
#1300 = ADVANCED_FACE ( 'NONE', ( #6079 ), #2003, .T. ) ;
#1301 =( LENGTH_UNIT ( ) NAMED_UNIT ( * ) SI_UNIT ( $, .METRE. ) );
#1302 = EDGE_CURVE ( 'NONE', #450, #3721, #3853, .T. ) ;
#1303 = CARTESIAN_POINT ( 'NONE',  ( 0.3543307086614173596, 0.000000000000000000, -0.4082677165354330340 ) ) ;
#1304 = B_SPLINE_CURVE_WITH_KNOTS ( 'NONE', 3,
 ( #742, #54, #1222, #4140, #7086, #4754, #7161, #2377, #3608, #6434, #3570, #6477, #1846, #4678, #4798, #5912, #3069, #6562 ),
 .UNSPECIFIED., .F., .F.,
 ( 4, 2, 2, 2, 2, 2, 2, 2, 4 ),
 ( 3.469446951953614189E-18, 0.0002327816859446636656, 0.0004655633718893238617, 0.0009311267437786459886, 0.001396690115667967953, 0.001862253487557290026, 0.002327816859446611882, 0.002793380231335934171, 0.003724506975114588291 ),
 .UNSPECIFIED. ) ;
#1305 = AXIS2_PLACEMENT_3D ( 'NONE', #5939, #4127, #3483 ) ;
#1306 = ORIENTED_EDGE ( 'NONE', *, *, #5383, .F. ) ;
#1307 = SHAPE_REPRESENTATION ( 'Link', ( #5166 ), #4787 ) ;
#1308 = ORIENTED_EDGE ( 'NONE', *, *, #389, .T. ) ;
#1309 = AXIS2_PLACEMENT_3D ( 'NONE', #5269, #4619, #4731 ) ;
#1310 =( LENGTH_UNIT ( ) NAMED_UNIT ( * ) SI_UNIT ( $, .METRE. ) );
#1311 = CARTESIAN_POINT ( 'NONE',  ( 0.3510872220067592364, -0.3295092824291515621, -0.01982436236955561690 ) ) ;
#1312 = CARTESIAN_POINT ( 'NONE',  ( -1.085749034322391227, 0.4630669964643871483, -1.535808346805855429 ) ) ;
#1313 = AXIS2_PLACEMENT_3D ( 'NONE', #762, #4930, #5931 ) ;
#1314 = CARTESIAN_POINT ( 'NONE',  ( 0.3581828924050327045, -0.3486337532542230222, -1.123169198254405176E-18 ) ) ;
#1315 = CARTESIAN_POINT ( 'NONE',  ( 1.205350347085700102, 0.08351947907094880996, -0.9807282671443031674 ) ) ;
#1316 = TOROIDAL_SURFACE ( 'NONE', #827, 1.223643328182681289, 0.05905511811023622659 ) ;
#1317 = CARTESIAN_POINT ( 'NONE',  ( -0.4445636273010806772, -1.003669596044584722, -1.568530023225017223 ) ) ;
#1318 = CARTESIAN_POINT ( 'NONE',  ( 0.4685039370078740717, 0.000000000000000000, 0.000000000000000000 ) ) ;
#1319 = TOROIDAL_SURFACE ( 'NONE', #6834, 0.4507874015748032370, 0.03543307086614166934 ) ;
#1320 = ITEM_DEFINED_TRANSFORMATION ( 'NONE', 'NONE', #2036,  #5166 ) ;
#1321 = CARTESIAN_POINT ( 'NONE',  ( 0.003035684155427131534, 0.2845908893795032757, 0.09762530132584859577 ) ) ;
#1322 = CARTESIAN_POINT ( 'NONE',  ( -0.1922007978147441398, -0.2981786776988375465, -2.347681869555223892E-17 ) ) ;
#1323 = CARTESIAN_POINT ( 'NONE',  ( 1.649606299212598381, 0.000000000000000000, 0.1982677165354330695 ) ) ;
#1324 = CARTESIAN_POINT ( 'NONE',  ( 2.755905511811024056, 1.496062992125984259, 0.000000000000000000 ) ) ;
#1325 = EDGE_LOOP ( 'NONE', ( #6231, #4106 ) ) ;
#1326 = CARTESIAN_POINT ( 'NONE',  ( 2.892866454678787531E-17, 1.496062992125984259, 0.2362204724409449341 ) ) ;
#1327 = DIRECTION ( 'NONE',  ( 1.000000000000000000, 0.000000000000000000, 0.000000000000000000 ) ) ;
#1328 = VECTOR ( 'NONE', #1791, 39.37007874015748143 ) ;
#1329 = VERTEX_POINT ( 'NONE', #5509 ) ;
#1330 = CARTESIAN_POINT ( 'NONE',  ( 0.7511002112796222319, -0.03873617871155973086, 0.9835188775901014813 ) ) ;
#1331 = CIRCLE ( 'NONE', #6599, 1.968503937007874072 ) ;
#1332 = CARTESIAN_POINT ( 'NONE',  ( 0.4330708661417322913, 1.048552902599920289, -1.573978973432616835 ) ) ;
#1333 = VERTEX_POINT ( 'NONE', #420 ) ;
#1334 = CARTESIAN_POINT ( 'NONE',  ( 0.4476001829033102175, 0.9971724964169970118, -1.429776958199368675 ) ) ;
#1335 = EDGE_LOOP ( 'NONE', ( #1893, #4756, #2974, #5553, #2259 ) ) ;
#1336 = EDGE_CURVE ( 'NONE', #733, #3843, #3029, .T. ) ;
#1337 = ORIENTED_EDGE ( 'NONE', *, *, #459, .F. ) ;
#1338 = CARTESIAN_POINT ( 'NONE',  ( 0.3403864257300625029, -0.2851194846584945153, -0.09670974744601064377 ) ) ;
#1339 = CARTESIAN_POINT ( 'NONE',  ( 0.3505601438611543053, -0.3409548833797009237, 1.488710258487716964E-17 ) ) ;
#1340 = CARTESIAN_POINT ( 'NONE',  ( -0.4339190921229451603, -0.9541934910893047350, -1.456692913385828625 ) ) ;
#1341 = CIRCLE ( 'NONE', #2215, 1.968503937007874072 ) ;
#1342 = LENGTH_MEASURE_WITH_UNIT ( LENGTH_MEASURE( 0.02539999999999999897 ), #7503 );
#1343 = EDGE_CURVE ( 'NONE', #772, #1258, #2850, .T. ) ;
#1344 = ORIENTED_EDGE ( 'NONE', *, *, #1880, .F. ) ;
#1345 = ADVANCED_FACE ( 'NONE', ( #2588 ), #3837, .T. ) ;
#1346 = AXIS2_PLACEMENT_3D ( 'NONE', #1462, #7321, #4349 ) ;
#1347 = LENGTH_MEASURE_WITH_UNIT ( LENGTH_MEASURE( 0.02539999999999999897 ), #4227 );
#1348 = PRODUCT_DEFINITION_SHAPE ( 'NONE', 'NONE',  #7546 ) ;
#1349 = EDGE_CURVE ( 'NONE', #5600, #1896, #6775, .T. ) ;
#1350 = CARTESIAN_POINT ( 'NONE',  ( 0.3543307086614173040, 0.1714946277491099791, -0.02209865905065017816 ) ) ;
#1351 = LENGTH_MEASURE_WITH_UNIT ( LENGTH_MEASURE( 0.02539999999999999897 ), #1769 );
#1352 = AXIS2_PLACEMENT_3D ( 'NONE', #2242, #3305, #4001 ) ;
#1353 = CARTESIAN_POINT ( 'NONE',  ( 0.5141614760841459741, -1.056523642887403192, -1.484898342931014303 ) ) ;
#1354 = AXIS2_PLACEMENT_3D ( 'NONE', #769, #3136, #4515 ) ;
#1355 = ADVANCED_FACE ( 'NONE', ( #6334 ), #2851, .F. ) ;
#1356 = UNCERTAINTY_MEASURE_WITH_UNIT (LENGTH_MEASURE( 1.000000000000000082E-05 ), #1698, 'distance_accuracy_value', 'NONE');
#1357 = CARTESIAN_POINT ( 'NONE',  ( 0.02637295201093751290, -0.3409548833797009237, -9.138209691400258722E-18 ) ) ;
#1358 = CARTESIAN_POINT ( 'NONE',  ( 0.05817553349160910214, 0.3755582001340100340, -0.01402797064541879898 ) ) ;
#1359 = AXIS2_PLACEMENT_3D ( 'NONE', #2959, #2852, #5225 ) ;
#1360 = DIRECTION ( 'NONE',  ( -0.000000000000000000, -1.000000000000000000, -0.000000000000000000 ) ) ;
#1361 = CARTESIAN_POINT ( 'NONE',  ( 0.3425764178929367465, 0.2322094954269895706, -0.2008802154383052541 ) ) ;
#1362 = CARTESIAN_POINT ( 'NONE',  ( -1.651526287078852914E-15, 0.000000000000000000, -1.456692913385827515 ) ) ;
#1363 = CARTESIAN_POINT ( 'NONE',  ( 0.000000000000000000, 2.957312202238506242E-17, 0.2952755905511810774 ) ) ;
#1364 = CARTESIAN_POINT ( 'NONE',  ( 2.755905511811024056, 1.496062992125984259, 0.7480314960629921295 ) ) ;
#1365 = ORIENTED_EDGE ( 'NONE', *, *, #7283, .T. ) ;
#1366 = DIRECTION ( 'NONE',  ( -1.000000000000000000, -0.000000000000000000, -0.000000000000000000 ) ) ;
#1367 = CARTESIAN_POINT ( 'NONE',  ( -0.5141614760841456411, 1.056523642887403414, -1.484898342931014303 ) ) ;
#1368 = AXIS2_PLACEMENT_3D ( 'NONE', #1690, #1654, #4602 ) ;
#1369 = EDGE_LOOP ( 'NONE', ( #1958, #2983, #132, #1571, #1534, #6317 ) ) ;
#1370 = DIRECTION ( 'NONE',  ( -0.000000000000000000, -1.000000000000000000, -0.000000000000000000 ) ) ;
#1371 = CARTESIAN_POINT ( 'NONE',  ( 0.3403868552871069930, -0.05881191477760600722, -0.2952755905511810774 ) ) ;
#1372 = CARTESIAN_POINT ( 'NONE',  ( 0.7556634140584972403, -0.06154568813258620014, 0.9824437959648022467 ) ) ;
#1373 = TOROIDAL_SURFACE ( 'NONE', #3455, 0.4507874015748032370, 0.03543307086614166934 ) ;
#1374 = PLANE ( 'NONE',  #7171 ) ;
#1375 = ORIENTED_EDGE ( 'NONE', *, *, #4398, .F. ) ;
#1376 = CARTESIAN_POINT ( 'NONE',  ( 0.3321022367507226458, 0.2411754471855206694, -0.1728230530388957520 ) ) ;
#1377 = B_SPLINE_CURVE_WITH_KNOTS ( 'NONE', 3,
 ( #5855, #4562, #2866, #5719, #2831, #2295 ),
 .UNSPECIFIED., .F., .F.,
 ( 4, 2, 4 ),
 ( 2.380730968220726014E-07, 0.002629065763328353091, 0.005257893453559884557 ),
 .UNSPECIFIED. ) ;
#1378 = VERTEX_POINT ( 'NONE', #4645 ) ;
#1379 = ORIENTED_EDGE ( 'NONE', *, *, #1767, .T. ) ;
#1380 = CARTESIAN_POINT ( 'NONE',  ( 0.000000000000000000, -0.2557161625347748601, 0.1476377952755911216 ) ) ;
#1381 = PRESENTATION_STYLE_ASSIGNMENT (( #6633 ) ) ;
#1382 = CARTESIAN_POINT ( 'NONE',  ( 0.9921524035015079068, -0.4406690496059638140, -1.439080679658372608 ) ) ;
#1383 = VERTEX_POINT ( 'NONE', #4076 ) ;
#1384 = CARTESIAN_POINT ( 'NONE',  ( 0.8062609481994166272, 0.1560654929534785462, 0.9718629971449804783 ) ) ;
#1385 = AXIS2_PLACEMENT_3D ( 'NONE', #2670, #956, #2632 ) ;
#1386 = LINE ( 'NONE', #5541, #6967 ) ;
#1387 = CONICAL_SURFACE ( 'NONE', #439, 0.1982677165354330695, 0.7853981633974452814 ) ;
#1388 = VERTEX_POINT ( 'NONE', #5165 ) ;
#1389 = AXIS2_PLACEMENT_3D ( 'NONE', #7168, #6647, #4270 ) ;
#1390 = CARTESIAN_POINT ( 'NONE',  ( 0.004822332172886080806, 0.2197023059474403073, -0.2100156246613533173 ) ) ;
#1391 = CARTESIAN_POINT ( 'NONE',  ( 1.102581283201567564, -0.2050316615124324060, -0.9626998336838916703 ) ) ;
#1392 = EDGE_CURVE ( 'NONE', #4697, #3247, #1627, .T. ) ;
#1393 = CARTESIAN_POINT ( 'NONE',  ( 0.4996352642496096341, -1.070877820178676831, -1.498503547059352403 ) ) ;
#1394 = PRESENTATION_LAYER_ASSIGNMENT (  '', '', ( #5694 ) ) ;
#1395 = DIRECTION ( 'NONE',  ( 1.000000000000000000, 0.000000000000000000, 2.095133389269358970E-15 ) ) ;
#1396 = PLANE ( 'NONE',  #1949 ) ;
#1397 = ADVANCED_FACE ( 'NONE', ( #3618 ), #7475, .F. ) ;
#1398 = CARTESIAN_POINT ( 'NONE',  ( -0.2520187439128739881, -0.2636427704167116359, -0.005786797686151756714 ) ) ;
#1399 = FACE_OUTER_BOUND ( 'NONE', #7029, .T. ) ;
#1400 = ADVANCED_FACE ( 'NONE', ( #5224 ), #2249, .F. ) ;
#1401 = ORIENTED_EDGE ( 'NONE', *, *, #3232, .F. ) ;
#1402 = CARTESIAN_POINT ( 'NONE',  ( -0.4330708661417316807, 1.051607560569806088, -1.573502278225820561 ) ) ;
#1403 = ORIENTED_EDGE ( 'NONE', *, *, #3403, .F. ) ;
#1404 = CARTESIAN_POINT ( 'NONE',  ( 0.000000000000000000, 1.496062992125984259, 0.000000000000000000 ) ) ;
#1405 = FACE_OUTER_BOUND ( 'NONE', #7413, .T. ) ;
#1406 = DIRECTION ( 'NONE',  ( -1.000000000000000000, 0.000000000000000000, -0.000000000000000000 ) ) ;
#1407 = ORIENTED_EDGE ( 'NONE', *, *, #5673, .F. ) ;
#1408 = CARTESIAN_POINT ( 'NONE',  ( 0.3403864257301138507, 0.2263128404110440195, -0.1985658431051529893 ) ) ;
#1409 = VERTEX_POINT ( 'NONE', #597 ) ;
#1410 = ORIENTED_EDGE ( 'NONE', *, *, #5003, .F. ) ;
#1411 = DIRECTION ( 'NONE',  ( 0.000000000000000000, 0.000000000000000000, -1.000000000000000000 ) ) ;
#1412 = AXIS2_PLACEMENT_3D ( 'NONE', #4879, #2131, #4422 ) ;
#1413 = DIRECTION ( 'NONE',  ( -1.000000000000000000, -0.000000000000000000, -0.000000000000000000 ) ) ;
#1414 = ORIENTED_EDGE ( 'NONE', *, *, #1251, .F. ) ;
#1415 = ORIENTED_EDGE ( 'NONE', *, *, #3600, .T. ) ;
#1416 = CARTESIAN_POINT ( 'NONE',  ( -0.3543307086614173040, -0.1372236123666514263, -0.3942809247306748865 ) ) ;
#1417 = EDGE_LOOP ( 'NONE', ( #658, #5953, #7045, #4091 ) ) ;
#1418 =( NAMED_UNIT ( * ) PLANE_ANGLE_UNIT ( ) SI_UNIT ( $, .RADIAN. ) );
#1419 = VERTEX_POINT ( 'NONE', #6944 ) ;
#1420 =( CONVERSION_BASED_UNIT ( 'INCH', #1347 ) LENGTH_UNIT ( ) NAMED_UNIT ( #5712 ) );
#1421 = VECTOR ( 'NONE', #2082, 39.37007874015748143 ) ;
#1422 = FACE_OUTER_BOUND ( 'NONE', #6071, .T. ) ;
#1423 = FACE_OUTER_BOUND ( 'NONE', #4511, .T. ) ;
#1424 = AXIS2_PLACEMENT_3D ( 'NONE', #4083, #5203, #5846 ) ;
#1425 = ADVANCED_FACE ( 'NONE', ( #3432, #1665 ), #7437, .T. ) ;
#1426 = CARTESIAN_POINT ( 'NONE',  ( 5.766273211944702482E-30, -1.651526287078852914E-15, -1.456692913385827515 ) ) ;
#1427 = B_SPLINE_CURVE_WITH_KNOTS ( 'NONE', 3,
 ( #510, #471, #1518, #2673, #2716, #5173, #6888, #3864, #3906, #4477, #5091, #5677, #7484, #390, #2258, #6238, #4554, #3330 ),
 .UNSPECIFIED., .F., .F.,
 ( 4, 2, 2, 2, 2, 2, 2, 2, 4 ),
 ( 0.000000000000000000, 0.0002385177155853649095, 0.0004770354311707298190, 0.0009540708623414807799, 0.001431106293512231795, 0.001908141724682982810, 0.002385177155853733608, 0.002862212587024484840, 0.003816283449365995978 ),
 .UNSPECIFIED. ) ;
#1428 = CARTESIAN_POINT ( 'NONE',  ( 0.3391892065151630442, 0.3125419764313920878, -0.04921259842519681155 ) ) ;
#1429 = VECTOR ( 'NONE', #5394, 39.37007874015748143 ) ;
#1430 = DIRECTION ( 'NONE',  ( 0.000000000000000000, 0.000000000000000000, -1.000000000000000000 ) ) ;
#1431 = CARTESIAN_POINT ( 'NONE',  ( 0.9861598787149247203, 0.4544645342395175480, -1.560495034967182670 ) ) ;
#1432 = ORIENTED_EDGE ( 'NONE', *, *, #2059, .T. ) ;
#1433 = CARTESIAN_POINT ( 'NONE',  ( -0.9697097640641210159, 0.4330708661417288496, -1.453662949853142594 ) ) ;
#1434 = CARTESIAN_POINT ( 'NONE',  ( 0.1771653543307089296, -0.3068593950417301541, -0.4082677165354330340 ) ) ;
#1435 = APPLICATION_CONTEXT ( 'automotive_design' ) ;
#1436 = AXIS2_PLACEMENT_3D ( 'NONE', #4183, #2419, #4711 ) ;
#1437 = LINE ( 'NONE', #2140, #5071 ) ;
#1438 = EDGE_CURVE ( 'NONE', #1762, #2951, #3304, .T. ) ;
#1439 = EDGE_CURVE ( 'NONE', #2064, #4413, #4934, .T. ) ;
#1440 = DIRECTION ( 'NONE',  ( 0.000000000000000000, 0.000000000000000000, -1.000000000000000000 ) ) ;
#1441 = EDGE_CURVE ( 'NONE', #5853, #4821, #460, .T. ) ;
#1442 = CARTESIAN_POINT ( 'NONE',  ( 0.4589126309195376008, 1.085572762089311416, -1.540322683979783669 ) ) ;
#1443 = ORIENTED_EDGE ( 'NONE', *, *, #484, .F. ) ;
#1444 = CIRCLE ( 'NONE', #6462, 0.2362204724409449619 ) ;
#1445 = CARTESIAN_POINT ( 'NONE',  ( 4.536176542591472873E-15, -0.4330708661417322913, -2.204724409448820754 ) ) ;
#1446 = ORIENTED_EDGE ( 'NONE', *, *, #3413, .T. ) ;
#1447 = ORIENTED_EDGE ( 'NONE', *, *, #4387, .T. ) ;
#1448 = CARTESIAN_POINT ( 'NONE',  ( 0.02637295201093723881, -0.1704774416898505729, -0.2952755905511810774 ) ) ;
#1449 = AXIS2_PLACEMENT_3D ( 'NONE', #6996, #617, #3452 ) ;
#1450 = LINE ( 'NONE', #4906, #6203 ) ;
#1451 = CARTESIAN_POINT ( 'NONE',  ( 0.9726684123052360409, -0.4332839571663233968, -1.452651065350215154 ) ) ;
#1452 = ORIENTED_EDGE ( 'NONE', *, *, #6784, .T. ) ;
#1453 = CARTESIAN_POINT ( 'NONE',  ( 0.8280287984149673486, 0.1778526427332735582, 0.9681128863842415333 ) ) ;
#1454 = ORIENTED_EDGE ( 'NONE', *, *, #6089, .T. ) ;
#1455 = VERTEX_POINT ( 'NONE', #5737 ) ;
#1456 = ORIENTED_EDGE ( 'NONE', *, *, #2885, .T. ) ;
#1457 = CARTESIAN_POINT ( 'NONE',  ( 0.000000000000000000, 0.000000000000000000, 0.000000000000000000 ) ) ;
#1458 = CARTESIAN_POINT ( 'NONE',  ( 1.611653543307086212, 0.000000000000000000, 0.000000000000000000 ) ) ;
#1459 = CARTESIAN_POINT ( 'NONE',  ( 1.145762533245342940, -0.1725491722722915233, -0.9690247371578599722 ) ) ;
#1460 = CARTESIAN_POINT ( 'NONE',  ( -0.9479499796399307732, -0.4353079511162269433, -1.456692913385828625 ) ) ;
#1461 = CARTESIAN_POINT ( 'NONE',  ( 1.102718734937994105, 0.2049554913489460561, -0.9627163727494573164 ) ) ;
#1462 = CARTESIAN_POINT ( 'NONE',  ( 0.000000000000000000, 0.2699662542182227343, 0.1783464566929134354 ) ) ;
#1463 = CARTESIAN_POINT ( 'NONE',  ( 5.942930443104038687E-30, -1.702122929023921893E-15, -1.433776001880363582 ) ) ;
#1464 = AXIS2_PLACEMENT_3D ( 'NONE', #2510, #3665, #1395 ) ;
#1465 = DIRECTION ( 'NONE',  ( 0.000000000000000000, 0.000000000000000000, 1.000000000000000000 ) ) ;
#1466 = DIRECTION ( 'NONE',  ( -1.000000000000000000, 0.000000000000000000, 0.000000000000000000 ) ) ;
#1467 = DIRECTION ( 'NONE',  ( 1.047444401652940007E-14, -1.000000000000000000, 0.000000000000000000 ) ) ;
#1468 = ORIENTED_EDGE ( 'NONE', *, *, #5382, .F. ) ;
#1469 = PRODUCT_DEFINITION_SHAPE ( 'NONE', 'NONE',  #787 ) ;
#1470 = CARTESIAN_POINT ( 'NONE',  ( -0.9960023578760586194, 0.4720886891211098502, -1.401719942879699143 ) ) ;
#1471 = EDGE_CURVE ( 'NONE', #4570, #5600, #4405, .T. ) ;
#1472 = AXIS2_PLACEMENT_3D ( 'NONE', #2508, #7205, #3813 ) ;
#1473 =( GEOMETRIC_REPRESENTATION_CONTEXT ( 3 ) GLOBAL_UNCERTAINTY_ASSIGNED_CONTEXT ( ( #5340 ) ) GLOBAL_UNIT_ASSIGNED_CONTEXT ( ( #4919, #4836, #824 ) ) REPRESENTATION_CONTEXT ( 'NONE', 'WORKASPACE' ) );
#1474 = CARTESIAN_POINT ( 'NONE',  ( -0.1470270249832137943, 0.3242597676034320586, -0.0007480297793123595346 ) ) ;
#1475 = CARTESIAN_POINT ( 'NONE',  ( 0.3496779450092586949, 0.1779791412978203036, -0.2952755905511810774 ) ) ;
#1476 = CIRCLE ( 'NONE', #5168, 0.05944881889763781874 ) ;
#1477 = ITEM_DEFINED_TRANSFORMATION ( 'NONE', 'NONE', #394,  #5166 ) ;
#1478 = CARTESIAN_POINT ( 'NONE',  ( 0.4470331066954957855, 1.081428707249768140, -1.553789012478534959 ) ) ;
#1479 = ORIENTED_EDGE ( 'NONE', *, *, #900, .T. ) ;
#1480 = TOROIDAL_SURFACE ( 'NONE', #2470, 1.043121362164705745, 0.05905511811023622659 ) ;
#1481 = DIRECTION ( 'NONE',  ( 0.000000000000000000, 0.000000000000000000, -1.000000000000000000 ) ) ;
#1482 = EDGE_CURVE ( 'NONE', #725, #7262, #3582, .T. ) ;
#1483 = EDGE_CURVE ( 'NONE', #1950, #7325, #2210, .T. ) ;
#1484 = VERTEX_POINT ( 'NONE', #6265 ) ;
#1485 = EDGE_LOOP ( 'NONE', ( #4566, #4218, #6459, #3058, #1131, #2751 ) ) ;
#1486 = EDGE_CURVE ( 'NONE', #5632, #1005, #4075, .T. ) ;
#1487 = CIRCLE ( 'NONE', #5898, 1.168853328413309134 ) ;
#1488 = DIRECTION ( 'NONE',  ( 0.000000000000000000, -1.000000000000000000, 0.000000000000000000 ) ) ;
#1489 = DIRECTION ( 'NONE',  ( 0.000000000000000000, 0.000000000000000000, -1.000000000000000000 ) ) ;
#1490 = CARTESIAN_POINT ( 'NONE',  ( 0.0006233585804809438748, -0.2412158484082067011, 0.1727530760685163091 ) ) ;
#1491 = CARTESIAN_POINT ( 'NONE',  ( 0.9990286721055837704, -0.4596436929058785315, -1.415369458146013004 ) ) ;
#1492 = VERTEX_POINT ( 'NONE', #5959 ) ;
#1493 = CARTESIAN_POINT ( 'NONE',  ( 0.9997522001112967294, 0.2362259618796917759, 0.9554837688155867204 ) ) ;
#1494 = EDGE_CURVE ( 'NONE', #6698, #4990, #6605, .T. ) ;
#1495 = ORIENTED_EDGE ( 'NONE', *, *, #144, .T. ) ;
#1496 = EDGE_CURVE ( 'NONE', #655, #6130, #7017, .T. ) ;
#1497 = VECTOR ( 'NONE', #3502, 39.37007874015748143 ) ;
#1498 = PRESENTATION_STYLE_ASSIGNMENT (( #5816 ) ) ;
#1499 = ORIENTED_EDGE ( 'NONE', *, *, #1018, .T. ) ;
#1500 = DIRECTION ( 'NONE',  ( 0.8813569915457180048, 0.4724509005743148249, -9.318298004224719768E-17 ) ) ;
#1501 = CARTESIAN_POINT ( 'NONE',  ( 0.3483227611829848303, -0.1704774416898505729, -0.2952755905511810774 ) ) ;
#1502 = CARTESIAN_POINT ( 'NONE',  ( 0.0006233585804807679088, 0.2412158484082065346, -0.1727530760685158651 ) ) ;
#1503 = AXIS2_PLACEMENT_3D ( 'NONE', #3855, #378, #6113 ) ;
#1504 = COLOUR_RGB ( '',0.7921568627450980005, 0.8196078431372548767, 0.9333333333333333481 ) ;
#1505 = CARTESIAN_POINT ( 'NONE',  ( 0.8226608724162054465, 0.1724771829768798059, -0.9690378908208601150 ) ) ;
#1506 = VECTOR ( 'NONE', #831, 39.37007874015748143 ) ;
#1507 = LENGTH_MEASURE_WITH_UNIT ( LENGTH_MEASURE( 0.02539999999999999897 ), #7504 );
#1508 = CARTESIAN_POINT ( 'NONE',  ( 0.9842519685039370358, 1.220472440944881942, 0.4724409448818898127 ) ) ;
#1509 = CARTESIAN_POINT ( 'NONE',  ( 2.892866454678787531E-17, 0.000000000000000000, 0.2362204724409449341 ) ) ;
#1510 = CARTESIAN_POINT ( 'NONE',  ( -0.4368380215374121356, 1.023371766162644914, -1.573834103987475475 ) ) ;
#1511 = ORIENTED_EDGE ( 'NONE', *, *, #2020, .T. ) ;
#1512 = CARTESIAN_POINT ( 'NONE',  ( 0.000000000000000000, 0.000000000000000000, -0.4082677165354330340 ) ) ;
#1513 = VERTEX_POINT ( 'NONE', #60 ) ;
#1514 = CARTESIAN_POINT ( 'NONE',  ( -0.4330708661417317362, -1.048552902599920955, -1.573978973432617279 ) ) ;
#1515 = CARTESIAN_POINT ( 'NONE',  ( 0.01836325778988931109, -0.1427310470019619582, -0.2952755905511810774 ) ) ;
#1516 = APPLICATION_PROTOCOL_DEFINITION ( 'draft international standard', 'automotive_design', 1998, #5621 ) ;
#1517 = MANIFOLD_SOLID_BREP ( 'Cut-Extrude1', #6528 ) ;
#1518 = CARTESIAN_POINT ( 'NONE',  ( -0.9726683636255518683, -0.4332839536939438463, -1.452651081959920987 ) ) ;
#1519 = ORIENTED_EDGE ( 'NONE', *, *, #4662, .T. ) ;
#1520 = CARTESIAN_POINT ( 'NONE',  ( 1.060348520640345571, -0.4341579107161988582, -1.570964845243104424 ) ) ;
#1521 = FACE_OUTER_BOUND ( 'NONE', #5793, .T. ) ;
#1522 = EDGE_LOOP ( 'NONE', ( #7339, #2572, #3193, #6564, #6097, #5636 ) ) ;
#1523 = EDGE_LOOP ( 'NONE', ( #5727, #547, #165, #442 ) ) ;
#1524 = FACE_OUTER_BOUND ( 'NONE', #2237, .T. ) ;
#1525 = ADVANCED_FACE ( 'NONE', ( #4721 ), #7053, .F. ) ;
#1526 = DIRECTION ( 'NONE',  ( 1.000000000000000000, 0.000000000000000000, 0.000000000000000000 ) ) ;
#1527 = ORIENTED_EDGE ( 'NONE', *, *, #7279, .F. ) ;
#1528 = CARTESIAN_POINT ( 'NONE',  ( 0.3465694189147047188, 0.3147628225698786419, 0.04536598007754604617 ) ) ;
#1529 = VERTEX_POINT ( 'NONE', #6035 ) ;
#1530 = CARTESIAN_POINT ( 'NONE',  ( 0.3483227611829848303, -0.1704774416898505729, -0.2952755905511810774 ) ) ;
#1531 = VERTEX_POINT ( 'NONE', #3076 ) ;
#1532 = CARTESIAN_POINT ( 'NONE',  ( 0.3409812221349194372, 0.2754857644942527717, 0.1258275564122752488 ) ) ;
#1533 = ORIENTED_EDGE ( 'NONE', *, *, #6781, .F. ) ;
#1534 = ORIENTED_EDGE ( 'NONE', *, *, #4718, .T. ) ;
#1535 = LINE ( 'NONE', #2772, #2357 ) ;
#1536 = EDGE_CURVE ( 'NONE', #1079, #5576, #215, .T. ) ;
#1537 = EDGE_CURVE ( 'NONE', #1603, #6545, #2213, .T. ) ;
#1538 = DIRECTION ( 'NONE',  ( 0.8340899802306024347, -0.5516284119576448930, 2.280240126189561055E-16 ) ) ;
#1539 = DIRECTION ( 'NONE',  ( 0.000000000000000000, 0.000000000000000000, 1.000000000000000000 ) ) ;
#1540 = DIRECTION ( 'NONE',  ( 1.000000000000000000, 0.000000000000000000, 0.000000000000000000 ) ) ;
#1541 = CARTESIAN_POINT ( 'NONE',  ( 0.9685300475558180633, -0.2358242948353262147, -0.9555833128140062138 ) ) ;
#1542 = EDGE_CURVE ( 'NONE', #662, #1296, #1625, .T. ) ;
#1543 = CARTESIAN_POINT ( 'NONE',  ( -0.3543307086614173040, 0.2045729300278205931, -0.3766201741223081378 ) ) ;
#1544 = CARTESIAN_POINT ( 'NONE',  ( 1.089060247968624440, 0.2122540722833457794, -0.9611122372014845316 ) ) ;
#1545 = MANIFOLD_SOLID_BREP ( 'FlangeHexFillet', #4204 ) ;
#1546 = CARTESIAN_POINT ( 'NONE',  ( 0.4416276115803088875, 1.010073413237866147, -1.570717210673254538 ) ) ;
#1547 = B_SPLINE_CURVE_WITH_KNOTS ( 'NONE', 3,
 ( #1704, #2313, #2279, #5810, #2256, #1027, #1059, #4513, #6377 ),
 .UNSPECIFIED., .F., .F.,
 ( 4, 2, 1, 2, 4 ),
 ( 0.000000000000000000, 0.002165063509461094028, 0.004330127018922188056, 0.006495190528383282084, 0.008660254037844376113 ),
 .UNSPECIFIED. ) ;
#1548 = CARTESIAN_POINT ( 'NONE',  ( 0.3505601438611538057, 0.1704774416898496292, -0.2952755905511812995 ) ) ;
#1549 = CARTESIAN_POINT ( 'NONE',  ( 7.874015748031496287, 0.2559055118110236116, -0.2362204724409455170 ) ) ;
#1550 = CIRCLE ( 'NONE', #2536, 0.2362204724409449619 ) ;
#1551 = CARTESIAN_POINT ( 'NONE',  ( 2.755905511811024056, 1.496062992125984259, -0.2362204724409449896 ) ) ;
#1552 = SHAPE_REPRESENTATION ( 'hex flange bolt small_iso_ISO 4162 - M12 x 65 x 65-N', ( #5166 ), #1726 ) ;
#1553 = ORIENTED_EDGE ( 'NONE', *, *, #5622, .F. ) ;
#1554 = FACE_BOUND ( 'NONE', #1577, .T. ) ;
#1555 = DIRECTION ( 'NONE',  ( 0.000000000000000000, 0.000000000000000000, -1.000000000000000000 ) ) ;
#1556 = CIRCLE ( 'NONE', #4730, 0.2362204724409448231 ) ;
#1557 = CONTEXT_DEPENDENT_SHAPE_REPRESENTATION ( #4336, #3808 ) ;
#1558 = MANIFOLD_SOLID_BREP ( 'Boss-Extrude2', #7369 ) ;
#1559 = CARTESIAN_POINT ( 'NONE',  ( 0.3336175750056034062, -0.2273032555864673288, -0.1968503937007873295 ) ) ;
#1560 = EDGE_LOOP ( 'NONE', ( #6936, #5410, #1956, #5814 ) ) ;
#1561 = CARTESIAN_POINT ( 'NONE',  ( 0.000000000000000000, -0.2557161625347750822, -0.1476377952755907330 ) ) ;
#1562 = DIRECTION ( 'NONE',  ( -0.000000000000000000, -0.000000000000000000, 1.000000000000000000 ) ) ;
#1563 = VECTOR ( 'NONE', #1988, 39.37007874015748143 ) ;
#1564 = B_SPLINE_CURVE_WITH_KNOTS ( 'NONE', 3,
 ( #2083, #3222, #2608, #7306, #5495, #290 ),
 .UNSPECIFIED., .F., .F.,
 ( 4, 2, 4 ),
 ( 2.380730968505120768E-07, 0.002629065763328379546, 0.005257893453559907976 ),
 .UNSPECIFIED. ) ;
#1565 = VERTEX_POINT ( 'NONE', #1622 ) ;
#1566 = EDGE_LOOP ( 'NONE', ( #2501, #4241, #1650, #7410, #2975, #4490, #6140 ) ) ;
#1567 = SPHERICAL_SURFACE ( 'NONE', #530, 1.259842519685039131 ) ;
#1568 = CARTESIAN_POINT ( 'NONE',  ( 0.9773775067402629135, 0.4999746636856571835, -1.373988502838980885 ) ) ;
#1569 = CIRCLE ( 'NONE', #5359, 1.174991162294038771 ) ;
#1570 = CARTESIAN_POINT ( 'NONE',  ( 0.002513486811083624848, -0.2845799557467911245, 0.09764423893321799719 ) ) ;
#1571 = ORIENTED_EDGE ( 'NONE', *, *, #1681, .T. ) ;
#1572 = DIRECTION ( 'NONE',  ( 0.000000000000000000, -0.000000000000000000, 1.000000000000000000 ) ) ;
#1573 = ORIENTED_EDGE ( 'NONE', *, *, #603, .T. ) ;
#1574 = CARTESIAN_POINT ( 'NONE',  ( 1.220472440944881720, -1.984939871850715226E-17, 0.9842519685039370358 ) ) ;
#1575 = CARTESIAN_POINT ( 'NONE',  ( 0.3531511627980717938, 0.3349346966101464096, 0.02350890366534340997 ) ) ;
#1576 = EDGE_CURVE ( 'NONE', #4172, #2074, #2775, .T. ) ;
#1577 = EDGE_LOOP ( 'NONE', ( #4101, #786 ) ) ;
#1578 = CIRCLE ( 'NONE', #3909, 1.223643328182683065 ) ;
#1579 = FACE_OUTER_BOUND ( 'NONE', #5139, .T. ) ;
#1580 = CARTESIAN_POINT ( 'NONE',  ( 26.63278072698489396, 34.81515369617522992, 51.43712309129124094 ) ) ;
#1581 = CARTESIAN_POINT ( 'NONE',  ( 0.3527006543068525457, -0.1709223289430796822, -0.2960461578774135627 ) ) ;
#1582 = CARTESIAN_POINT ( 'NONE',  ( 0.9411660957780360048, 0.4368170150760492532, -1.456692913385828847 ) ) ;
#1583 = CARTESIAN_POINT ( 'NONE',  ( -0.9479499796399307732, -0.4353079511162269433, -1.456692913385828625 ) ) ;
#1584 = AXIS2_PLACEMENT_3D ( 'NONE', #5075, #6531, #3616 ) ;
#1585 = ADVANCED_FACE ( 'NONE', ( #1732 ), #1316, .T. ) ;
#1586 = DIRECTION ( 'NONE',  ( 0.000000000000000000, 0.000000000000000000, 1.000000000000000000 ) ) ;
#1587 = ADVANCED_FACE ( 'NONE', ( #3461 ), #1387, .T. ) ;
#1588 = EDGE_CURVE ( 'NONE', #5110, #3761, #6867, .T. ) ;
#1589 = EDGE_CURVE ( 'NONE', #4488, #4463, #7305, .T. ) ;
#1590 =( REPRESENTATION_RELATIONSHIP ('NONE','NONE', #303, #5265 ) REPRESENTATION_RELATIONSHIP_WITH_TRANSFORMATION ( #6004 )SHAPE_REPRESENTATION_RELATIONSHIP( ) );
#1591 = CARTESIAN_POINT ( 'NONE',  ( 0.3528971332113847725, -0.1886393090946611450, -0.2768874834731246404 ) ) ;
#1592 = CARTESIAN_POINT ( 'NONE',  ( 0.3411151615605706455, -0.2917056203871725706, 0.09774174715353350917 ) ) ;
#1593 = CARTESIAN_POINT ( 'NONE',  ( 0.01834252172841645614, 0.3270457701237517445, 0.02409129084753309363 ) ) ;
#1594 = CIRCLE ( 'NONE', #867, 0.2362204724409449341 ) ;
#1595 = DIRECTION ( 'NONE',  ( -2.207829878515936732E-15, 0.000000000000000000, 1.000000000000000000 ) ) ;
#1596 = EDGE_CURVE ( 'NONE', #1, #3631, #4215, .T. ) ;
#1597 = VERTEX_POINT ( 'NONE', #3493 ) ;
#1598 = CARTESIAN_POINT ( 'NONE',  ( -0.8884031170519980369, 0.4627498550472156080, -1.439912866901231547 ) ) ;
#1599 = CARTESIAN_POINT ( 'NONE',  ( 0.9604263920613221872, -0.4330708661417219663, -1.456063616177414310 ) ) ;
#1600 = CIRCLE ( 'NONE', #2703, 1.168853328413308690 ) ;
#1601 = CONTEXT_DEPENDENT_SHAPE_REPRESENTATION ( #5516, #1911 ) ;
#1602 = CARTESIAN_POINT ( 'NONE',  ( -0.4921259842519648542, 0.000000000000000000, -2.204724409448822975 ) ) ;
#1603 = VERTEX_POINT ( 'NONE', #5079 ) ;
#1604 = CARTESIAN_POINT ( 'NONE',  ( 0.3391216574608371670, 0.3159523085418723398, -0.04330572993916122215 ) ) ;
#1605 = CARTESIAN_POINT ( 'NONE',  ( 0.3565422270302656127, -0.1673297761639321035, 0.3007275071673038980 ) ) ;
#1606 =( BOUNDED_SURFACE ( )  B_SPLINE_SURFACE ( 3, 2, ( 
 ( #2453, #6024, #3104 ),
 ( #175, #5322, #2533 ),
 ( #1888, #3726, #3024 ),
 ( #3144, #4335, #3642 ),
 ( #6557, #1338, #3061 ),
 ( #2498, #5907, #6064 ),
 ( #6668, #4830, #4178 ),
 ( #7156, #7189, #1297 ) ),
 .UNSPECIFIED., .F., .F., .F. ) 
 B_SPLINE_SURFACE_WITH_KNOTS ( ( 4, 2, 2, 4 ),
 ( 3, 3 ),
 ( 0.03551798592901340978, 0.03994769179990649566, 0.04216254473535303859, 0.04437739767079958153 ),
 ( 0.000000000000000000, 1.000000000000000000 ),
 .UNSPECIFIED. ) 
 GEOMETRIC_REPRESENTATION_ITEM ( )  RATIONAL_B_SPLINE_SURFACE ( (
 ( 1.000000000000000000, 0.8047781103519396906, 1.000000000000000000),
 ( 1.000000000000000000, 0.8123785826170297764, 1.000000000000000000),
 ( 1.000000000000000000, 0.8190671539034730664, 1.000000000000000000),
 ( 1.000000000000000000, 0.8191932076449999212, 1.000000000000000000),
 ( 1.000000000000000000, 0.8176085094066802839, 1.000000000000000000),
 ( 1.000000000000000000, 0.8122955484013585359, 1.000000000000000000),
 ( 1.000000000000000000, 0.8086308001281159452, 1.000000000000000000),
 ( 1.000000000000000000, 0.8047712537969721192, 1.000000000000000000) ) ) 
 REPRESENTATION_ITEM ( '' )  SURFACE ( )  );
#1607 = VERTEX_POINT ( 'NONE', #3647 ) ;
#1608 = VECTOR ( 'NONE', #2840, 39.37007874015748143 ) ;
#1609 = ORIENTED_EDGE ( 'NONE', *, *, #6825, .F. ) ;
#1610 = CARTESIAN_POINT ( 'NONE',  ( 0.8403423717953923955, -0.1874820019069840249, 0.9662438517680175254 ) ) ;
#1611 = CARTESIAN_POINT ( 'NONE',  ( 21.65354330708661479, 0.000000000000000000, 0.4921259842519685179 ) ) ;
#1612 = AXIS2_PLACEMENT_3D ( 'NONE', #5740, #6304, #5167 ) ;
#1613 = ORIENTED_EDGE ( 'NONE', *, *, #3137, .F. ) ;
#1614 = DIRECTION ( 'NONE',  ( -1.000000000000000000, 0.000000000000000000, 0.000000000000000000 ) ) ;
#1615 = ORIENTED_EDGE ( 'NONE', *, *, #842, .T. ) ;
#1616 = DIRECTION ( 'NONE',  ( 0.000000000000000000, 0.000000000000000000, 1.000000000000000000 ) ) ;
#1617 = EDGE_LOOP ( 'NONE', ( #5149, #4373, #767, #6843, #2822, #4828 ) ) ;
#1618 = CIRCLE ( 'NONE', #28, 0.1982677165354330695 ) ;
#1619 = ORIENTED_EDGE ( 'NONE', *, *, #613, .T. ) ;
#1620 = DIRECTION ( 'NONE',  ( 0.8672889550420763705, -0.4978050506594157154, -1.508467848325716170E-30 ) ) ;
#1621 = DIRECTION ( 'NONE',  ( 1.000000000000000000, 0.000000000000000000, 0.000000000000000000 ) ) ;
#1622 = CARTESIAN_POINT ( 'NONE',  ( 0.000000000000000000, 0.000000000000000000, 0.7480314960629921295 ) ) ;
#1623 = AXIS2_PLACEMENT_3D ( 'NONE', #6268, #1669, #2253 ) ;
#1624 = FACE_OUTER_BOUND ( 'NONE', #2746, .T. ) ;
#1625 = CIRCLE ( 'NONE', #907, 0.3543307086614173596 ) ;
#1626 = EDGE_CURVE ( 'NONE', #283, #7001, #6146, .T. ) ;
#1627 = LINE ( 'NONE', #4611, #6643 ) ;
#1628 = CARTESIAN_POINT ( 'NONE',  ( -0.2362204724409449619, 0.000000000000000000, -0.4072677165354330331 ) ) ;
#1629 = CARTESIAN_POINT ( 'NONE',  ( 1.279527559055118280, 1.968503937007874072, 0.4724409448818898127 ) ) ;
#1630 = CARTESIAN_POINT ( 'NONE',  ( 2.755905511811024056, 0.000000000000000000, 0.000000000000000000 ) ) ;
#1631 = TOROIDAL_SURFACE ( 'NONE', #6768, 1.124634398195722973, 0.05905511811023622659 ) ;
#1632 = ORIENTED_EDGE ( 'NONE', *, *, #7103, .T. ) ;
#1633 = CARTESIAN_POINT ( 'NONE',  ( 0.4637690556582351187, -0.9984401429152542917, -1.410743228759550050 ) ) ;
#1634 = CARTESIAN_POINT ( 'NONE',  ( 0.3581828924050327045, -0.3486337532542230222, -1.123169198254405176E-18 ) ) ;
#1635 = CARTESIAN_POINT ( 'NONE',  ( -2.349015779708382802E-16, 0.2702383257424525453, -0.1224846707640857985 ) ) ;
#1636 = ADVANCED_FACE ( 'NONE', ( #5328 ), #1891, .F. ) ;
#1637 = ITEM_DEFINED_TRANSFORMATION ( 'NONE', 'NONE', #6621,  #5166 ) ;
#1638 = B_SPLINE_CURVE_WITH_KNOTS ( 'NONE', 3,
 ( #320, #355, #5524, #4859, #2037, #4364, #2603, #244 ),
 .UNSPECIFIED., .F., .F.,
 ( 4, 2, 2, 4 ),
 ( -7.690028535483255933E-06, 0.001102852776893270938, 0.001658124179607644699, 0.002213395582322018676 ),
 .UNSPECIFIED. ) ;
#1639 = EDGE_CURVE ( 'NONE', #7488, #6858, #2662, .T. ) ;
#1640 = AXIS2_PLACEMENT_3D ( 'NONE', #2692, #5654, #2509 ) ;
#1641 = CARTESIAN_POINT ( 'NONE',  ( 0.000000000000000000, 0.000000000000000000, -0.4921259842519685179 ) ) ;
#1642 = ORIENTED_EDGE ( 'NONE', *, *, #2250, .F. ) ;
#1644 = CARTESIAN_POINT ( 'NONE',  ( -0.5141614760841456411, 1.056523642887403414, -1.484898342931014303 ) ) ;
#1643 = DIMENSIONAL_EXPONENTS ( 1.000000000000000000, 0.000000000000000000, 0.000000000000000000, 0.000000000000000000, 0.000000000000000000, 0.000000000000000000, 0.000000000000000000 ) ;
#1645 = CYLINDRICAL_SURFACE ( 'NONE', #4436, 0.2362204724409449619 ) ;
#1646 = ORIENTED_EDGE ( 'NONE', *, *, #3657, .F. ) ;
#1647 = ORIENTED_EDGE ( 'NONE', *, *, #603, .F. ) ;
#1648 = CARTESIAN_POINT ( 'NONE',  ( 0.8592737258235019215, -0.2005978551774719454, 0.9636033532647499955 ) ) ;
#1649 = CARTESIAN_POINT ( 'NONE',  ( 0.3581828924050324825, 0.3486337532542225226, 1.056976728655274672E-17 ) ) ;
#1650 = ORIENTED_EDGE ( 'NONE', *, *, #2285, .F. ) ;
#1651 = B_SPLINE_CURVE_WITH_KNOTS ( 'NONE', 3,
 ( #6002, #1235, #5840, #6571 ),
 .UNSPECIFIED., .F., .F.,
 ( 4, 4 ),
 ( 0.000000000000000000, 0.0004815725036528541126 ),
 .UNSPECIFIED. ) ;
#1652 = DIRECTION ( 'NONE',  ( -0.000000000000000000, -1.000000000000000000, 0.000000000000000000 ) ) ;
#1653 = ORIENTED_EDGE ( 'NONE', *, *, #986, .F. ) ;
#1654 = DIRECTION ( 'NONE',  ( 0.000000000000000000, 0.000000000000000000, -1.000000000000000000 ) ) ;
#1655 = ORIENTED_EDGE ( 'NONE', *, *, #6907, .T. ) ;
#1656 = ORIENTED_EDGE ( 'NONE', *, *, #4450, .T. ) ;
#1657 = CYLINDRICAL_SURFACE ( 'NONE', #4910, 0.4724409448818896462 ) ;
#1658 = DIRECTION ( 'NONE',  ( -0.5516284119576448930, -0.8340899802306024347, -6.479022119375340223E-17 ) ) ;
#1659 = FACE_BOUND ( 'NONE', #6578, .T. ) ;
#1660 = CARTESIAN_POINT ( 'NONE',  ( -0.9541934910893034028, -0.4339190921229485465, -1.456692913385828847 ) ) ;
#1661 = CARTESIAN_POINT ( 'NONE',  ( 0.3527008206095850196, -0.1709223649093223885, 0.2960462201727743770 ) ) ;
#1662 = CARTESIAN_POINT ( 'NONE',  ( 0.1469816153540864645, 0.3242859848650325727, -0.4082677165354333115 ) ) ;
#1663 = FACE_OUTER_BOUND ( 'NONE', #6270, .T. ) ;
#1664 =( CONVERSION_BASED_UNIT ( 'INCH', #4579 ) LENGTH_UNIT ( ) NAMED_UNIT ( #2768 ) );
#1665 = FACE_OUTER_BOUND ( 'NONE', #5827, .T. ) ;
#1666 = FACE_OUTER_BOUND ( 'NONE', #580, .T. ) ;
#1667 = DIRECTION ( 'NONE',  ( -1.000000000000000000, -1.047444401652940007E-14, -6.779428194327236205E-32 ) ) ;
#1668 = UNCERTAINTY_MEASURE_WITH_UNIT (LENGTH_MEASURE( 1.000000000000000082E-05 ), #5254, 'distance_accuracy_value', 'NONE');
#1669 = DIRECTION ( 'NONE',  ( 2.207829878515936732E-15, -0.000000000000000000, -1.000000000000000000 ) ) ;
#1670 = EDGE_CURVE ( 'NONE', #1248, #10, #6582, .T. ) ;
#1671 = DIRECTION ( 'NONE',  ( 0.000000000000000000, 0.000000000000000000, -1.000000000000000000 ) ) ;
#1672 = CARTESIAN_POINT ( 'NONE',  ( 0.4377664870282949594, -0.9883299873891294718, -1.443420526770071044 ) ) ;
#1673 = DIRECTION ( 'NONE',  ( -1.000000000000000000, 0.000000000000000000, -0.000000000000000000 ) ) ;
#1674 = CONTEXT_DEPENDENT_SHAPE_REPRESENTATION ( #4715, #3059 ) ;
#1675 = FACE_OUTER_BOUND ( 'NONE', #1522, .T. ) ;
#1676 = CYLINDRICAL_SURFACE ( 'NONE', #7190, 0.2362204724409449341 ) ;
#1677 = EDGE_LOOP ( 'NONE', ( #6252, #2486, #6667, #6069 ) ) ;
#1678 = DIRECTION ( 'NONE',  ( 0.000000000000000000, 0.000000000000000000, -1.000000000000000000 ) ) ;
#1679 = CARTESIAN_POINT ( 'NONE',  ( 0.3321022367507227568, -0.2411754471855062087, 0.1728230530389214537 ) ) ;
#1680 = EDGE_CURVE ( 'NONE', #2401, #358, #1221, .T. ) ;
#1681 = EDGE_CURVE ( 'NONE', #3999, #929, #2570, .T. ) ;
#1682 = CIRCLE ( 'NONE', #2408, 0.9842519685039370358 ) ;
#1683 = VERTEX_POINT ( 'NONE', #1798 ) ;
#1684 = DIRECTION ( 'NONE',  ( -1.000000000000000000, -0.000000000000000000, -0.000000000000000000 ) ) ;
#1685 = ADVANCED_FACE ( 'NONE', ( #2376 ), #3027, .T. ) ;
#1686 = FILL_AREA_STYLE_COLOUR ( '', #5223 ) ;
#1687 = CARTESIAN_POINT ( 'NONE',  ( -2.834645669291338432, 0.000000000000000000, 2.952755905511811108 ) ) ;
#1688 = VERTEX_POINT ( 'NONE', #7041 ) ;
#1689 = CIRCLE ( 'NONE', #1796, 0.2952755905511810774 ) ;
#1690 = CARTESIAN_POINT ( 'NONE',  ( 0.000000000000000000, 0.000000000000000000, -1.515748031496062964 ) ) ;
#1691 = VERTEX_POINT ( 'NONE', #2990 ) ;
#1692 =( REPRESENTATION_RELATIONSHIP ('NONE','NONE', #303, #785 ) REPRESENTATION_RELATIONSHIP_WITH_TRANSFORMATION ( #2534 )SHAPE_REPRESENTATION_RELATIONSHIP( ) );
#1693 = FACE_OUTER_BOUND ( 'NONE', #89, .T. ) ;
#1694 = CIRCLE ( 'NONE', #2191, 0.2699662542182227343 ) ;
#1695 =( NAMED_UNIT ( * ) SI_UNIT ( $, .STERADIAN. ) SOLID_ANGLE_UNIT ( ) );
#1696 = CIRCLE ( 'NONE', #4748, 0.2952755905511810774 ) ;
#1697 = DIRECTION ( 'NONE',  ( 0.000000000000000000, 0.000000000000000000, 1.000000000000000000 ) ) ;
#1698 =( CONVERSION_BASED_UNIT ( 'INCH', #2914 ) LENGTH_UNIT ( ) NAMED_UNIT ( #7497 ) );
#1699 = CIRCLE ( 'NONE', #1449, 1.074277634097406953 ) ;
#1700 = CARTESIAN_POINT ( 'NONE',  ( -0.3543307086614173040, 0.000000000000000000, 7.886165872636028972E-17 ) ) ;
#1701 = DIRECTION ( 'NONE',  ( 0.000000000000000000, 1.000000000000000000, 0.000000000000000000 ) ) ;
#1702 = CARTESIAN_POINT ( 'NONE',  ( 0.3565422129079688918, -0.1767726971815447856, -0.2952755905511810774 ) ) ;
#1703 = COLOUR_RGB ( '',0.7921568627450980005, 0.8196078431372548767, 0.9333333333333333481 ) ;
#1704 = CARTESIAN_POINT ( 'NONE',  ( 0.3483227611829846637, -0.1704774416898499345, 0.2952755905511811330 ) ) ;
#1705 = CARTESIAN_POINT ( 'NONE',  ( 7.714310545810097206E-17, 0.000000000000000000, -0.9448818897637817349 ) ) ;
#1706 = CARTESIAN_POINT ( 'NONE',  ( -0.4843356560173193159, -0.9895441027518994126, -1.389133886014304320 ) ) ;
#1707 = ORIENTED_EDGE ( 'NONE', *, *, #1247, .F. ) ;
#1708 = CARTESIAN_POINT ( 'NONE',  ( -2.834645669291338432, 0.4724409448818898127, 0.4724409448818898127 ) ) ;
#1709 = DIRECTION ( 'NONE',  ( -1.000000000000000000, 0.000000000000000000, 0.000000000000000000 ) ) ;
#1710 = ORIENTED_EDGE ( 'NONE', *, *, #3316, .T. ) ;
#1711 = VECTOR ( 'NONE', #6176, 39.37007874015748143 ) ;
#1712 = ORIENTED_EDGE ( 'NONE', *, *, #6995, .T. ) ;
#1713 = CARTESIAN_POINT ( 'NONE',  ( 0.000000000000000000, 0.000000000000000000, 0.000000000000000000 ) ) ;
#1714 = ADVANCED_FACE ( 'NONE', ( #5416 ), #3714, .F. ) ;
#1715 = FACE_OUTER_BOUND ( 'NONE', #7164, .T. ) ;
#1716 = ADVANCED_FACE ( 'NONE', ( #2458 ), #5735, .T. ) ;
#1717 = EDGE_LOOP ( 'NONE', ( #3998, #4981, #7337, #692 ) ) ;
#1718 = AXIS2_PLACEMENT_3D ( 'NONE', #1190, #3537, #5873 ) ;
#1719 = CARTESIAN_POINT ( 'NONE',  ( 1.140074190135267118, 0.1777047106289595946, 0.9680897379949867654 ) ) ;
#1720 = B_SPLINE_CURVE_WITH_KNOTS ( 'NONE', 3,
 ( #6704, #2682, #2043, #4337 ),
 .UNSPECIFIED., .F., .F.,
 ( 4, 4 ),
 ( 0.000000000000000000, 0.0002807012396509386419 ),
 .UNSPECIFIED. ) ;
#1721 = VECTOR ( 'NONE', #7379, 39.37007874015748143 ) ;
#1722 = CARTESIAN_POINT ( 'NONE',  ( 0.000000000000000000, 0.000000000000000000, -0.7480314960629921295 ) ) ;
#1723 = ADVANCED_FACE ( 'NONE', ( #5951 ), #5843, .T. ) ;
#1724 = ORIENTED_EDGE ( 'NONE', *, *, #2492, .F. ) ;
#1725 = CONICAL_SURFACE ( 'NONE', #3322, 0.3543307086614173596, 1.047197551196596521 ) ;
#1726 =( GEOMETRIC_REPRESENTATION_CONTEXT ( 3 ) GLOBAL_UNCERTAINTY_ASSIGNED_CONTEXT ( ( #3116 ) ) GLOBAL_UNIT_ASSIGNED_CONTEXT ( ( #4344, #1897, #5502 ) ) REPRESENTATION_CONTEXT ( 'NONE', 'WORKASPACE' ) );
#1727 = CARTESIAN_POINT ( 'NONE',  ( 0.4685039370078740717, -0.3409548833797009237, 0.000000000000000000 ) ) ;
#1728 = DIRECTION ( 'NONE',  ( 1.000000000000000000, 0.000000000000000000, 0.000000000000000000 ) ) ;
#1729 = EDGE_CURVE ( 'NONE', #135, #7001, #237, .T. ) ;
#1730 = CARTESIAN_POINT ( 'NONE',  ( 0.4685039370078740717, 0.3409548833797004797, 0.000000000000000000 ) ) ;
#1731 = EDGE_CURVE ( 'NONE', #1683, #2077, #1564, .T. ) ;
#1732 = FACE_OUTER_BOUND ( 'NONE', #6506, .T. ) ;
#1733 = DIRECTION ( 'NONE',  ( -0.000000000000000000, 0.000000000000000000, -1.000000000000000000 ) ) ;
#1734 = VECTOR ( 'NONE', #850, 39.37007874015748143 ) ;
#1735 = CARTESIAN_POINT ( 'NONE',  ( 0.4685039370078740717, 0.1704774416898497680, -0.2952755905511810774 ) ) ;
#1736 = DIRECTION ( 'NONE',  ( 0.000000000000000000, 0.000000000000000000, 1.000000000000000000 ) ) ;
#1737 = CYLINDRICAL_SURFACE ( 'NONE', #6153, 0.2362204724409449341 ) ;
#1738 = COLOUR_RGB ( '',0.7921568627450980005, 0.8196078431372548767, 0.9333333333333333481 ) ;
#1739 = CARTESIAN_POINT ( 'NONE',  ( 0.3505602286436571013, 0.1704774416898499345, 0.2952755905511810774 ) ) ;
#1740 = DIRECTION ( 'NONE',  ( 1.000000000000000000, 3.505805126173554996E-15, 0.000000000000000000 ) ) ;
#1741 = FACE_OUTER_BOUND ( 'NONE', #5613, .T. ) ;
#1742 = ORIENTED_EDGE ( 'NONE', *, *, #1392, .T. ) ;
#1743 = VECTOR ( 'NONE', #5300, 39.37007874015748143 ) ;
#1744 = DIRECTION ( 'NONE',  ( 0.000000000000000000, 1.000000000000000000, -2.193342766891360832E-15 ) ) ;
#1745 = DIRECTION ( 'NONE',  ( -1.000000000000000000, 0.000000000000000000, 0.000000000000000000 ) ) ;
#1746 = ORIENTED_EDGE ( 'NONE', *, *, #4312, .T. ) ;
#1747 = AXIS2_PLACEMENT_3D ( 'NONE', #2218, #5089, #6950 ) ;
#1748 = CARTESIAN_POINT ( 'NONE',  ( 2.989606299212598017, 2.892866454678787531E-17, -0.2362204724409449064 ) ) ;
#1749 = CARTESIAN_POINT ( 'NONE',  ( 0.3410425348215777031, 0.2759054741781710729, -0.1251041708914593098 ) ) ;
#1750 = ORIENTED_EDGE ( 'NONE', *, *, #339, .T. ) ;
#1751 = CARTESIAN_POINT ( 'NONE',  ( 0.4377665650305637701, 0.9883301303667320070, -1.443420399700354739 ) ) ;
#1752 = CYLINDRICAL_SURFACE ( 'NONE', #3778, 0.2362204724409448231 ) ;
#1753 = ORIENTED_EDGE ( 'NONE', *, *, #7332, .T. ) ;
#1754 = EDGE_CURVE ( 'NONE', #5614, #5707, #4950, .T. ) ;
#1755 = LINE ( 'NONE', #2241, #3814 ) ;
#1756 = CARTESIAN_POINT ( 'NONE',  ( 1.279527559055118280, 1.968503937007874072, 2.952755905511811108 ) ) ;
#1757 = CARTESIAN_POINT ( 'NONE',  ( 18.41860179314716817, 41.48855051017370243, 51.90956403617311565 ) ) ;
#1758 = CARTESIAN_POINT ( 'NONE',  ( 0.3543307086614173040, 0.1714946277491099791, -0.3861690574847828072 ) ) ;
#1759 = EDGE_LOOP ( 'NONE', ( #5817, #3961, #7254, #2648, #1443 ) ) ;
#1760 = CARTESIAN_POINT ( 'NONE',  ( 1.085749034841586580, -0.4630671888207288367, -1.535808138920397026 ) ) ;
#1761 = CARTESIAN_POINT ( 'NONE',  ( -0.4368170415251730332, -0.9411659768779440105, -1.456692913385828847 ) ) ;
#1762 = VERTEX_POINT ( 'NONE', #3799 ) ;
#1763 = PLANE ( 'NONE',  #2708 ) ;
#1764 = CARTESIAN_POINT ( 'NONE',  ( 0.7480314960629923515, 1.205359478595430764E-16, -0.9842519685039370358 ) ) ;
#1765 = EDGE_CURVE ( 'NONE', #1531, #4444, #4409, .T. ) ;
#1766 = ORIENTED_EDGE ( 'NONE', *, *, #3978, .T. ) ;
#1767 = EDGE_CURVE ( 'NONE', #3765, #383, #1186, .T. ) ;
#1768 = FACE_BOUND ( 'NONE', #1787, .T. ) ;
#1769 =( LENGTH_UNIT ( ) NAMED_UNIT ( * ) SI_UNIT ( $, .METRE. ) );
#1770 = DIRECTION ( 'NONE',  ( 1.000000000000000000, 0.000000000000000000, 0.000000000000000000 ) ) ;
#1771 = CARTESIAN_POINT ( 'NONE',  ( 0.3459458835994366765, 0.1200656956960832605, -0.2952755905511810774 ) ) ;
#1772 = AXIS2_PLACEMENT_3D ( 'NONE', #1843, #1142, #5323 ) ;
#1773 = PLANE ( 'NONE',  #7130 ) ;
#1774 = CARTESIAN_POINT ( 'NONE',  ( -0.4406690496059741946, 0.9921524035015047982, -1.439080679658375050 ) ) ;
#1775 = CARTESIAN_POINT ( 'NONE',  ( -1.641312181851277713E-15, 0.4700904924197903956, -2.204724409448820754 ) ) ;
#1776 = CONTEXT_DEPENDENT_SHAPE_REPRESENTATION ( #137, #7215 ) ;
#1777 = DIRECTION ( 'NONE',  ( 1.000000000000000000, 0.000000000000000000, 0.000000000000000000 ) ) ;
#1778 = DIRECTION ( 'NONE',  ( 1.000000000000000000, 0.000000000000000000, 0.000000000000000000 ) ) ;
#1779 = ORIENTED_EDGE ( 'NONE', *, *, #4207, .F. ) ;
#1780 = DIRECTION ( 'NONE',  ( -1.000000000000000000, -0.000000000000000000, -0.000000000000000000 ) ) ;
#1781 = CARTESIAN_POINT ( 'NONE',  ( 2.989606299212598017, 0.000000000000000000, 0.000000000000000000 ) ) ;
#1782 = ORIENTED_EDGE ( 'NONE', *, *, #2292, .F. ) ;
#1783 = EDGE_LOOP ( 'NONE', ( #1414, #6772, #424, #572 ) ) ;
#1784 = CARTESIAN_POINT ( 'NONE',  ( -0.2066929133858267931, 2.531258147843938473E-17, -0.3865922971001068409 ) ) ;
#1785=STYLED_ITEM('',(#7566),#4033);
#1786 = DIRECTION ( 'NONE',  ( -0.000000000000000000, -0.000000000000000000, 1.000000000000000000 ) ) ;
#1787 = EDGE_LOOP ( 'NONE', ( #5828, #2301 ) ) ;
#1788 = CARTESIAN_POINT ( 'NONE',  ( 0.4332839571663337774, 0.9726684123052319331, -1.452651065350215154 ) ) ;
#1789 = AXIS2_PLACEMENT_3D ( 'NONE', #1126, #7023, #2439 ) ;
#1790 = DIRECTION ( 'NONE',  ( 0.000000000000000000, 0.000000000000000000, 1.000000000000000000 ) ) ;
#1791 = DIRECTION ( 'NONE',  ( 1.000000000000000000, 0.000000000000000000, 0.000000000000000000 ) ) ;
#1792 = VERTEX_POINT ( 'NONE', #5607 ) ;
#1793 = FACE_BOUND ( 'NONE', #5066, .T. ) ;
#1794 = CARTESIAN_POINT ( 'NONE',  ( 0.3565422412058069090, 0.1767728485866832400, 0.2952755905511811330 ) ) ;
#1795 = DIRECTION ( 'NONE',  ( 0.000000000000000000, 0.000000000000000000, 1.000000000000000000 ) ) ;
#1796 = AXIS2_PLACEMENT_3D ( 'NONE', #6898, #3995, #5104 ) ;
#1797 = FILL_AREA_STYLE ('',( #4796 ) ) ;
#1798 = CARTESIAN_POINT ( 'NONE',  ( -9.561467977824920278E-16, -0.4091458600556405756, -0.03164754241312491001 ) ) ;
#1799 = ORIENTED_EDGE ( 'NONE', *, *, #97, .F. ) ;
#1800 = CARTESIAN_POINT ( 'NONE',  ( 2.989606299212598017, 0.000000000000000000, 0.2362204724409449064 ) ) ;
#1801 = ADVANCED_FACE ( 'NONE', ( #6102 ), #5769, .F. ) ;
#1802 = PLANE ( 'NONE',  #6018 ) ;
#1803 = CIRCLE ( 'NONE', #6100, 1.223643328182682621 ) ;
#1804 = VERTEX_POINT ( 'NONE', #3340 ) ;
#1805 = SHAPE_REPRESENTATION_RELATIONSHIP ( 'NONE' , 'NONE' ,  #1307, #6511 ) ;
#1806 = CARTESIAN_POINT ( 'NONE',  ( -0.4466261709646376366, 0.9159932075028757170, -1.451746187131335519 ) ) ;
#1807 = DIRECTION ( 'NONE',  ( -0.000000000000000000, -1.000000000000000000, -0.000000000000000000 ) ) ;
#1808 = CONICAL_SURFACE ( 'NONE', #7436, 0.3543307086614173596, 1.047197551196596521 ) ;
#1809 = ADVANCED_FACE ( 'NONE', ( #6857 ), #6816, .T. ) ;
#1810 = CARTESIAN_POINT ( 'NONE',  ( 0.3543307086614173596, -0.2045729300278204543, -0.3766201741223081378 ) ) ;
#1811 = EDGE_CURVE ( 'NONE', #1333, #2767, #2835, .T. ) ;
#1812 = CARTESIAN_POINT ( 'NONE',  ( 0.3388530074223801147, 0.06137376066181338130, -0.2952755905511810774 ) ) ;
#1813 = B_SPLINE_CURVE_WITH_KNOTS ( 'NONE', 3,
 ( #3089, #266, #836, #3780, #6114, #4319, #7212, #2483, #229, #2550 ),
 .UNSPECIFIED., .F., .F.,
 ( 4, 2, 2, 2, 4 ),
 ( 0.000000000000000000, 0.002239656411828510555, 0.004479312823657022845, 0.006718969235485534701, 0.008958625647314047424 ),
 .UNSPECIFIED. ) ;
#1814 = ADVANCED_FACE ( 'NONE', ( #7065, #3378, #4526 ), #6930, .T. ) ;
#1815 = AXIS2_PLACEMENT_3D ( 'NONE', #5943, #4864, #2076 ) ;
#1816 = PRODUCT_DEFINITION_CONTEXT ( 'detailed design', #5621, 'design' ) ;
#1817 = CARTESIAN_POINT ( 'NONE',  ( 0.3581828924050323715, 0.1743168766271109560, 0.3019256869348722616 ) ) ;
#1818 = LINE ( 'NONE', #4152, #3661 ) ;
#1819 = DIRECTION ( 'NONE',  ( -0.000000000000000000, -0.000000000000000000, 1.000000000000000000 ) ) ;
#1820 = ITEM_DEFINED_TRANSFORMATION ( 'NONE', 'NONE', #7031,  #5166 ) ;
#1821 = CARTESIAN_POINT ( 'NONE',  ( 0.4330708661417324024, 0.000000000000000000, 0.4507874015748032370 ) ) ;
#1822 = CARTESIAN_POINT ( 'NONE',  ( 0.3485616995351332181, 0.1165012447190262312, 0.3017003685801735724 ) ) ;
#1823 = CARTESIAN_POINT ( 'NONE',  ( -1.279527559055117836, 1.968503937007873850, 0.4724409448818898127 ) ) ;
#1824 = CARTESIAN_POINT ( 'NONE',  ( 0.4700904924197906176, 0.8785537298370117432, -1.433776001880362250 ) ) ;
#1825 = EDGE_CURVE ( 'NONE', #1529, #4777, #447, .T. ) ;
#1826 = ORIENTED_EDGE ( 'NONE', *, *, #3982, .T. ) ;
#1827 = CIRCLE ( 'NONE', #6347, 0.05944881889763779792 ) ;
#1828 = CARTESIAN_POINT ( 'NONE',  ( 0.3485534891173983629, 0.1164145375797932258, -0.3017001449125945034 ) ) ;
#1829 = CARTESIAN_POINT ( 'NONE',  ( 0.5118110236220474452, 1.220472440944881942, 2.480314960629921295 ) ) ;
#1830 = ORIENTED_EDGE ( 'NONE', *, *, #2207, .T. ) ;
#1831 = DIRECTION ( 'NONE',  ( 0.000000000000000000, 0.000000000000000000, 1.000000000000000000 ) ) ;
#1832 = APPLICATION_CONTEXT ( 'automotive_design' ) ;
#1833 = CARTESIAN_POINT ( 'NONE',  ( 0.3426404862726871725, 0.2904653615686527135, -0.09998168480679492376 ) ) ;
#1834 = ORIENTED_EDGE ( 'NONE', *, *, #4207, .T. ) ;
#1835 = CARTESIAN_POINT ( 'NONE',  ( 0.4330708661417322913, 0.000000000000000000, -2.204724409448820754 ) ) ;
#1836 = AXIS2_PLACEMENT_3D ( 'NONE', #7027, #1206, #3630 ) ;
#1837 = DIRECTION ( 'NONE',  ( -0.000000000000000000, -0.000000000000000000, -1.000000000000000000 ) ) ;
#1838 = EDGE_LOOP ( 'NONE', ( #6235, #7309 ) ) ;
#1839 = PRODUCT_DEFINITION_SHAPE ( 'NONE', 'NONE',  #7532 ) ;
#1840 = EDGE_LOOP ( 'NONE', ( #595, #4326, #6030, #6207, #3019, #7426 ) ) ;
#1841 = FACE_OUTER_BOUND ( 'NONE', #4334, .T. ) ;
#1842 = CARTESIAN_POINT ( 'NONE',  ( 0.3409809061799574659, 0.02876216262209277050, 0.3014914394333951253 ) ) ;
#1843 = CARTESIAN_POINT ( 'NONE',  ( 26.63278072698489041, 34.81515369617522992, 54.15482368919913370 ) ) ;
#1844 = AXIS2_PLACEMENT_3D ( 'NONE', #1198, #3044, #643 ) ;
#1845 = CARTESIAN_POINT ( 'NONE',  ( 0.3510870379221574522, 0.1475852640829200257, 0.2952755905511810774 ) ) ;
#1846 = CARTESIAN_POINT ( 'NONE',  ( -1.083679103503826902, -0.4755998196564530378, -1.522578840002906997 ) ) ;
#1847 = LINE ( 'NONE', #707, #3775 ) ;
#1848 = ORIENTED_EDGE ( 'NONE', *, *, #2275, .T. ) ;
#1849 = UNCERTAINTY_MEASURE_WITH_UNIT (LENGTH_MEASURE( 1.000000000000000082E-05 ), #3109, 'distance_accuracy_value', 'NONE');
#1850 = CARTESIAN_POINT ( 'NONE',  ( 0.3485777078273626928, -0.3195689143662223120, 0.04989192643193118837 ) ) ;
#1851 = AXIS2_PLACEMENT_3D ( 'NONE', #5302, #6408, #1233 ) ;
#1852 = ORIENTED_EDGE ( 'NONE', *, *, #6180, .T. ) ;
#1853 = AXIS2_PLACEMENT_3D ( 'NONE', #6813, #3914, #359 ) ;
#1854 =( NAMED_UNIT ( * ) PLANE_ANGLE_UNIT ( ) SI_UNIT ( $, .RADIAN. ) );
#1855 = CARTESIAN_POINT ( 'NONE',  ( 0.3459463601586513781, -0.1956820507697304701, -0.2516199270400212851 ) ) ;
#1856 = FACE_OUTER_BOUND ( 'NONE', #5913, .T. ) ;
#1857 = CARTESIAN_POINT ( 'NONE',  ( -1.083679103503829788, 0.4755998196564457658, -1.522578840002907219 ) ) ;
#1858 = AXIS2_PLACEMENT_3D ( 'NONE', #638, #4722, #7054 ) ;
#1859 = CARTESIAN_POINT ( 'NONE',  ( 0.3531513458567848707, -0.1471090214728858203, -0.3018164116569697075 ) ) ;
#1860 = CARTESIAN_POINT ( 'NONE',  ( 1.214400861842334090, 0.05376942629958520597, -0.9828113691670130603 ) ) ;
#1861 = VECTOR ( 'NONE', #1780, 39.37007874015748143 ) ;
#1862 = CARTESIAN_POINT ( 'NONE',  ( -0.4617902729102595916, -0.9752011746066798770, -1.554226146211785009 ) ) ;
#1863 = EDGE_CURVE ( 'NONE', #7188, #7376, #520, .T. ) ;
#1864 = DIRECTION ( 'NONE',  ( 0.000000000000000000, 1.000000000000000000, 0.000000000000000000 ) ) ;
#1865 = CARTESIAN_POINT ( 'NONE',  ( 0.3391892065151629332, 0.1988903486381583818, 0.2460629921259842312 ) ) ;
#1866 = CARTESIAN_POINT ( 'NONE',  ( 1.063161309294315515, 0.4348450248026808906, -1.569784497862149797 ) ) ;
#1867 = PLANE ( 'NONE',  #4389 ) ;
#1868 = DIRECTION ( 'NONE',  ( -1.000000000000000000, 0.000000000000000000, 0.000000000000000000 ) ) ;
#1869 = CARTESIAN_POINT ( 'NONE',  ( 0.000000000000000000, 0.000000000000000000, -1.515748031496062964 ) ) ;
#1870 = DIRECTION ( 'NONE',  ( 1.000000000000000000, 0.000000000000000000, 0.000000000000000000 ) ) ;
#1871 = VERTEX_POINT ( 'NONE', #403 ) ;
#1872 = CONICAL_SURFACE ( 'NONE', #6269, 0.2362204724409449619, 0.9599310885968795892 ) ;
#1873 = CARTESIAN_POINT ( 'NONE',  ( -0.4332776154273894620, -1.054581703806071857, -1.572814851683856041 ) ) ;
#1874 = DIRECTION ( 'NONE',  ( 0.000000000000000000, 1.000000000000000000, 0.000000000000000000 ) ) ;
#1875 = ORIENTED_EDGE ( 'NONE', *, *, #3882, .F. ) ;
#1876 = EDGE_CURVE ( 'NONE', #96, #4697, #2543, .T. ) ;
#1877 = EDGE_CURVE ( 'NONE', #698, #2114, #3402, .T. ) ;
#1878 = PLANE ( 'NONE',  #6498 ) ;
#1879 = AXIS2_PLACEMENT_3D ( 'NONE', #1463, #3317, #4430 ) ;
#1880 = EDGE_CURVE ( 'NONE', #5498, #4759, #939, .T. ) ;
#1881 = CARTESIAN_POINT ( 'NONE',  ( 3.198568410424924124, 2.407012729153881203, 2.480314960629921295 ) ) ;
#1882 = VERTEX_POINT ( 'NONE', #3873 ) ;
#1883 = CARTESIAN_POINT ( 'NONE',  ( 0.4342019027940197673, 0.9783381746514249189, -1.450123259817208687 ) ) ;
#1884 = DIRECTION ( 'NONE',  ( 1.000000000000000000, 0.000000000000000000, -0.000000000000000000 ) ) ;
#1885 = ORIENTED_EDGE ( 'NONE', *, *, #2117, .F. ) ;
#1886 = AXIS2_PLACEMENT_3D ( 'NONE', #3173, #6088, #4397 ) ;
#1887 = ORIENTED_EDGE ( 'NONE', *, *, #1729, .F. ) ;
#1888 = CARTESIAN_POINT ( 'NONE',  ( 0.3322361761492684806, -0.2247851515112275766, -0.2012118778978489453 ) ) ;
#1889 = CARTESIAN_POINT ( 'NONE',  ( 0.000000000000000000, 0.000000000000000000, -0.4082677165354330340 ) ) ;
#1890 = APPLICATION_PROTOCOL_DEFINITION ( 'draft international standard', 'automotive_design', 1998, #1435 ) ;
#1891 = CYLINDRICAL_SURFACE ( 'NONE', #2298, 0.2066929133858267931 ) ;
#1892 = CARTESIAN_POINT ( 'NONE',  ( 1.056523642887408521, -0.5141614760841347609, -1.484898342931014303 ) ) ;
#1893 = ORIENTED_EDGE ( 'NONE', *, *, #1680, .F. ) ;
#1894 = DIRECTION ( 'NONE',  ( 2.204015539012438360E-32, 4.625929269271482167E-15, -1.000000000000000000 ) ) ;
#1895 = CARTESIAN_POINT ( 'NONE',  ( 0.000000000000000000, 0.2559055118110236116, 0.4921259842519685179 ) ) ;
#1896 = VERTEX_POINT ( 'NONE', #7492 ) ;
#1897 =( NAMED_UNIT ( * ) PLANE_ANGLE_UNIT ( ) SI_UNIT ( $, .RADIAN. ) );
#1898 = CARTESIAN_POINT ( 'NONE',  ( 0.000000000000000000, 0.000000000000000000, 0.000000000000000000 ) ) ;
#1899 = CARTESIAN_POINT ( 'NONE',  ( 0.7601650273709252836, -0.07630400123961592063, -0.9813937435533869325 ) ) ;
#1900 =( BOUNDED_SURFACE ( )  B_SPLINE_SURFACE ( 3, 2, ( 
 ( #4507, #2704, #7438 ),
 ( #2211, #7401, #421 ),
 ( #3974, #2173, #1592 ),
 ( #1021, #6266, #6303 ),
 ( #3240, #6840, #461 ),
 ( #3856, #2780, #4470 ),
 ( #6228, #5588, #3391 ),
 ( #5048, #5124, #4543 ) ),
 .UNSPECIFIED., .F., .F., .F. ) 
 B_SPLINE_SURFACE_WITH_KNOTS ( ( 4, 2, 2, 4 ),
 ( 3, 3 ),
 ( 0.03551798592901338203, 0.03994769179990646790, 0.04216254473535301084, 0.04437739767079956071 ),
 ( 0.000000000000000000, 1.000000000000000000 ),
 .UNSPECIFIED. ) 
 GEOMETRIC_REPRESENTATION_ITEM ( )  RATIONAL_B_SPLINE_SURFACE ( (
 ( 1.000000000000000000, 0.8047781103519389134, 1.000000000000000000),
 ( 1.000000000000000000, 0.8123785826170312196, 1.000000000000000000),
 ( 1.000000000000000000, 0.8190671539034724002, 1.000000000000000000),
 ( 1.000000000000000000, 0.8191932076449992550, 1.000000000000000000),
 ( 1.000000000000000000, 0.8176085094069774906, 1.000000000000000000),
 ( 1.000000000000000000, 0.8122955484010631055, 1.000000000000000000),
 ( 1.000000000000000000, 0.8086308001283356583, 1.000000000000000000),
 ( 1.000000000000000000, 0.8047712537969732294, 1.000000000000000000) ) ) 
 REPRESENTATION_ITEM ( '' )  SURFACE ( )  );
#1901 = CARTESIAN_POINT ( 'NONE',  ( 0.4330708661417323468, -1.051607547633158113, -1.573502280244651441 ) ) ;
#1902 = CARTESIAN_POINT ( 'NONE',  ( 1.189177986357916605, 0.1185041968903534776, -0.9771775582510943137 ) ) ;
#1903 = LINE ( 'NONE', #4767, #1259 ) ;
#1904 = CARTESIAN_POINT ( 'NONE',  ( 0.3432736861146659657, 0.1846838951640041582, 0.2706692913385826960 ) ) ;
#1905 = ITEM_DEFINED_TRANSFORMATION ( 'NONE', 'NONE', #6188,  #5166 ) ;
#1906 = DIRECTION ( 'NONE',  ( 0.000000000000000000, -0.000000000000000000, 1.000000000000000000 ) ) ;
#1907 = CARTESIAN_POINT ( 'NONE',  ( 0.3543307086614173596, -0.2045729300278204543, -0.03164754241312491001 ) ) ;
#1908 = CARTESIAN_POINT ( 'NONE',  ( 0.000000000000000000, 0.2559055118110236116, 0.4921259842519685179 ) ) ;
#1909 = FACE_OUTER_BOUND ( 'NONE', #3959, .T. ) ;
#1910 = ORIENTED_EDGE ( 'NONE', *, *, #7518, .F. ) ;
#1911 = PRODUCT_DEFINITION_SHAPE ( 'NONE', 'NONE',  #7537 ) ;
#1912 = CARTESIAN_POINT ( 'NONE',  ( 0.3483227611829849413, -0.3409548833797009237, 0.000000000000000000 ) ) ;
#1913 = CARTESIAN_POINT ( 'NONE',  ( 0.3485777078273626928, -0.3195689143662223120, 0.04989192643193118837 ) ) ;
#1914 = B_SPLINE_CURVE_WITH_KNOTS ( 'NONE', 3,
 ( #7445, #353, #2143, #1559, #1034, #6198, #6806, #3404, #5710 ),
 .UNSPECIFIED., .F., .F.,
 ( 4, 2, 1, 2, 4 ),
 ( 0.000000000000000000, 0.002165063509461096630, 0.004330127018922193260, 0.006495190528383289023, 0.008660254037844388256 ),
 .UNSPECIFIED. ) ;
#1915 = ORIENTED_EDGE ( 'NONE', *, *, #5532, .T. ) ;
#1916 = FACE_OUTER_BOUND ( 'NONE', #4742, .T. ) ;
#1917 = EDGE_LOOP ( 'NONE', ( #4560, #3806, #2596, #5450, #2322 ) ) ;
#1918 = DIRECTION ( 'NONE',  ( -2.312579046053608732E-29, 2.207829878515936732E-15, 1.000000000000000000 ) ) ;
#1919 = EDGE_CURVE ( 'NONE', #6629, #210, #310, .T. ) ;
#1920 = EDGE_CURVE ( 'NONE', #3692, #725, #1689, .T. ) ;
#1921 = DIRECTION ( 'NONE',  ( -1.000000000000000000, 0.000000000000000000, 0.000000000000000000 ) ) ;
#1922 = ORIENTED_EDGE ( 'NONE', *, *, #5334, .T. ) ;
#1923 = EDGE_LOOP ( 'NONE', ( #1885, #6288, #3217, #242 ) ) ;
#1924 = EDGE_CURVE ( 'NONE', #477, #7296, #4618, .T. ) ;
#1925 = CARTESIAN_POINT ( 'NONE',  ( 0.000000000000000000, 0.000000000000000000, 0.4921259842519685179 ) ) ;
#1926 = B_SPLINE_CURVE_WITH_KNOTS ( 'NONE', 3,
 ( #4725, #1739, #30, #5264, #2434, #1817 ),
 .UNSPECIFIED., .F., .F.,
 ( 4, 2, 4 ),
 ( 0.000000000000000000, 0.0001677595217559110904, 0.0003355190435118221809 ),
 .UNSPECIFIED. ) ;
#1927 = ITEM_DEFINED_TRANSFORMATION ( 'NONE', 'NONE', #400,  #5166 ) ;
#1928 = FILL_AREA_STYLE_COLOUR ( '', #1703 ) ;
#1929 = CARTESIAN_POINT ( 'NONE',  ( 0.3403859949404050012, 0.05880135802647309951, 0.2952755905511811330 ) ) ;
#1930 = CIRCLE ( 'NONE', #5474, 0.3543307086614173596 ) ;
#1931 = EDGE_CURVE ( 'NONE', #5648, #3371, #1075, .T. ) ;
#1932 = CARTESIAN_POINT ( 'NONE',  ( 0.3565325103478085289, 0.1673557731150444039, 0.3006824791271354158 ) ) ;
#1933 = ORIENTED_EDGE ( 'NONE', *, *, #3316, .F. ) ;
#1934 = CIRCLE ( 'NONE', #1309, 0.4724409448818896462 ) ;
#1935 = LINE ( 'NONE', #219, #6015 ) ;
#1936 = CARTESIAN_POINT ( 'NONE',  ( -0.4627498550472187722, 0.8884031170519979259, -1.439912866901233324 ) ) ;
#1937 = CARTESIAN_POINT ( 'NONE',  ( -0.9044344578135158352, -0.4526814320286502435, -1.447629106959918754 ) ) ;
#1938 = B_SPLINE_CURVE_WITH_KNOTS ( 'NONE', 3,
 ( #5001, #7251, #4885, #6718, #2625, #2023, #188, #4315, #1940 ),
 .UNSPECIFIED., .F., .F.,
 ( 4, 2, 1, 2, 4 ),
 ( 0.000000000000000000, 0.002165063509461094028, 0.004330127018922188056, 0.006495190528383282084, 0.008660254037844376113 ),
 .UNSPECIFIED. ) ;
#1939 = CARTESIAN_POINT ( 'NONE',  ( 0.3581828924050324825, -0.1743168766271116221, -0.3019256869348722061 ) ) ;
#1940 = CARTESIAN_POINT ( 'NONE',  ( 0.3483227611829846637, 0.1704774416898499345, 0.2952755905511810774 ) ) ;
#1941 = VECTOR ( 'NONE', #6500, 39.37007874015748143 ) ;
#1942 = CARTESIAN_POINT ( 'NONE',  ( 0.3485373078438441796, 0.2031105961982143382, -0.2516016230262507203 ) ) ;
#1943 = DIRECTION ( 'NONE',  ( 5.296894631669315808E-46, -1.000000000000000000, 2.207829878515936732E-15 ) ) ;
#1944 = DIRECTION ( 'NONE',  ( -0.000000000000000000, -0.000000000000000000, 1.000000000000000000 ) ) ;
#1945 = CARTESIAN_POINT ( 'NONE',  ( 0.02637295201093703412, 0.1704774416898499345, 0.2952755905511810774 ) ) ;
#1946 = EDGE_LOOP ( 'NONE', ( #5786, #3725, #7037, #2047 ) ) ;
#1947 = CARTESIAN_POINT ( 'NONE',  ( -0.9921522615226839870, 0.4406689276647562936, -1.439080857166193717 ) ) ;
#1948 = CARTESIAN_POINT ( 'NONE',  ( 0.3581828924050324825, 0.3486337532542225226, 1.056976728655274672E-17 ) ) ;
#1949 = AXIS2_PLACEMENT_3D ( 'NONE', #4237, #3164, #3667 ) ;
#1950 = VERTEX_POINT ( 'NONE', #4733 ) ;
#1951 = CARTESIAN_POINT ( 'NONE',  ( 0.3510874053966554498, -0.1475872118127406207, -0.2952755905511810774 ) ) ;
#1952 = FACE_OUTER_BOUND ( 'NONE', #2722, .T. ) ;
#1953 = PRODUCT_DEFINITION ( 'UNKNOWN', '', #212, #5961 ) ;
#1954 = CIRCLE ( 'NONE', #7316, 0.2831409772408586822 ) ;
#1955 = DIRECTION ( 'NONE',  ( 1.000000000000000000, 0.000000000000000000, -0.000000000000000000 ) ) ;
#1956 = ORIENTED_EDGE ( 'NONE', *, *, #882, .F. ) ;
#1957 = CARTESIAN_POINT ( 'NONE',  ( 0.3496779274129792059, 0.3447056852546006578, 0.006496579416451838881 ) ) ;
#1958 = ORIENTED_EDGE ( 'NONE', *, *, #2885, .F. ) ;
#1959 = ORIENTED_EDGE ( 'NONE', *, *, #936, .T. ) ;
#1960 = CARTESIAN_POINT ( 'NONE',  ( 0.000000000000000000, 0.000000000000000000, -0.7983802283864780414 ) ) ;
#1961 = EDGE_CURVE ( 'NONE', #813, #1208, #970, .T. ) ;
#1962 = ADVANCED_FACE ( 'NONE', ( #1399 ), #4870, .T. ) ;
#1963 = CARTESIAN_POINT ( 'NONE',  ( 0.3253487914207032761, -0.2213056477483782425, -0.02198690333287102797 ) ) ;
#1964 = ORIENTED_EDGE ( 'NONE', *, *, #5478, .T. ) ;
#1965 = CARTESIAN_POINT ( 'NONE',  ( 0.3321022367506963890, 0.2702568778840441777, 0.1224525375122600818 ) ) ;
#1966 = ORIENTED_EDGE ( 'NONE', *, *, #7151, .F. ) ;
#1967 = AXIS2_PLACEMENT_3D ( 'NONE', #574, #4493, #6821 ) ;
#1968 = CARTESIAN_POINT ( 'NONE',  ( -0.3543307086614173040, 0.000000000000000000, -0.4082677165354330340 ) ) ;
#1969 = ADVANCED_FACE ( 'NONE', ( #4848 ), #4380, .T. ) ;
#1970 = ORIENTED_EDGE ( 'NONE', *, *, #134, .T. ) ;
#1971 = CARTESIAN_POINT ( 'NONE',  ( 0.9842519685039370358, 0.000000000000000000, -1.377952755905512028 ) ) ;
#1972 = VERTEX_POINT ( 'NONE', #1824 ) ;
#1973 = AXIS2_PLACEMENT_3D ( 'NONE', #2354, #4769, #3622 ) ;
#1974 = EDGE_CURVE ( 'NONE', #3692, #7446, #2186, .T. ) ;
#1975 = EDGE_CURVE ( 'NONE', #6027, #1005, #3710, .T. ) ;
#1976 = PRODUCT_DEFINITION_SHAPE ( 'NONE', 'NONE',  #7535 ) ;
#1977 = DIRECTION ( 'NONE',  ( 0.000000000000000000, 0.000000000000000000, -1.000000000000000000 ) ) ;
#1978 = CARTESIAN_POINT ( 'NONE',  ( 0.9079010304997725544, -0.2240813082648737964, -0.9584242268600799974 ) ) ;
#1979 = CARTESIAN_POINT ( 'NONE',  ( 2.834645669291338432, 0.000000000000000000, 2.952755905511811108 ) ) ;
#1980 = AXIS2_PLACEMENT_3D ( 'NONE', #5484, #4282, #203 ) ;
#1981 = CARTESIAN_POINT ( 'NONE',  ( -0.4700904924197908397, 0.8785537298370134085, -1.433776001880364470 ) ) ;
#1982 = DIRECTION ( 'NONE',  ( -1.000000000000000000, 0.000000000000000000, 0.000000000000000000 ) ) ;
#1983 = AXIS2_PLACEMENT_3D ( 'NONE', #7476, #984, #2251 ) ;
#1984 = DIRECTION ( 'NONE',  ( 0.000000000000000000, 1.000000000000000000, 0.000000000000000000 ) ) ;
#1985 = FACE_OUTER_BOUND ( 'NONE', #4298, .T. ) ;
#1986 = CARTESIAN_POINT ( 'NONE',  ( 0.4330708661417322913, -1.048552902599920289, -1.573978973432616835 ) ) ;
#1987 = DIRECTION ( 'NONE',  ( -0.000000000000000000, -0.000000000000000000, 1.000000000000000000 ) ) ;
#1988 = DIRECTION ( 'NONE',  ( 0.000000000000000000, 0.000000000000000000, 1.000000000000000000 ) ) ;
#1989 = ORIENTED_EDGE ( 'NONE', *, *, #3880, .T. ) ;
#1990 = CARTESIAN_POINT ( 'NONE',  ( 0.000000000000000000, 1.496062992125984259, 0.4921259842519685179 ) ) ;
#1991 = CARTESIAN_POINT ( 'NONE',  ( -0.4341579107162092943, 1.060348520640341352, -1.570964845243104646 ) ) ;
#1992 = AXIS2_PLACEMENT_3D ( 'NONE', #5022, #2075, #7226 ) ;
#1993 =( REPRESENTATION_RELATIONSHIP ('NONE','NONE', #303, #1552 ) REPRESENTATION_RELATIONSHIP_WITH_TRANSFORMATION ( #3328 )SHAPE_REPRESENTATION_RELATIONSHIP( ) );
#1994 = ORIENTED_EDGE ( 'NONE', *, *, #1496, .T. ) ;
#1995 = CARTESIAN_POINT ( 'NONE',  ( 1.649606299212598381, 2.428079244293728657E-17, -0.1982677165354330695 ) ) ;
#1996 = DIRECTION ( 'NONE',  ( -0.000000000000000000, -1.000000000000000000, -0.000000000000000000 ) ) ;
#1997 = CIRCLE ( 'NONE', #5405, 0.2362204724409448231 ) ;
#1998 = CARTESIAN_POINT ( 'NONE',  ( 0.4330708661417320138, 0.9604263920613175243, -1.456063616177414310 ) ) ;
#1999 = ORIENTED_EDGE ( 'NONE', *, *, #5233, .F. ) ;
#2000 = DIRECTION ( 'NONE',  ( -0.000000000000000000, -1.000000000000000000, -0.000000000000000000 ) ) ;
#2001 = ORIENTED_EDGE ( 'NONE', *, *, #1754, .F. ) ;
#2002 = ORIENTED_EDGE ( 'NONE', *, *, #3456, .T. ) ;
#2003 = CONICAL_SURFACE ( 'NONE', #1503, 0.2952755905511810774, 1.047197551196600518 ) ;
#2004 = CARTESIAN_POINT ( 'NONE',  ( 0.8785537298370166281, -0.4700904924197814028, -1.433776001880362250 ) ) ;
#2005 = B_SPLINE_CURVE_WITH_KNOTS ( 'NONE', 3,
 ( #6997, #169, #4631, #5246, #7032, #1749, #1833, #6513, #6962, #4 ),
 .UNSPECIFIED., .F., .F.,
 ( 4, 2, 2, 2, 4 ),
 ( 0.000000000000000000, 0.002239656411828510989, 0.004479312823657021977, 0.006718969235485534701, 0.008958625647314047424 ),
 .UNSPECIFIED. ) ;
#2006 = LINE ( 'NONE', #5605, #6194 ) ;
#2007 = CARTESIAN_POINT ( 'NONE',  ( 0.3442723180356496160, 0.3299850069800976948, 0.01900038327686272982 ) ) ;
#2008 = ORIENTED_EDGE ( 'NONE', *, *, #7250, .T. ) ;
#2009 = CARTESIAN_POINT ( 'NONE',  ( 0.7690174846032691303, 0.09763972085202782258, 0.9794230103293317669 ) ) ;
#2010 = ORIENTED_EDGE ( 'NONE', *, *, #3978, .F. ) ;
#2011 = CONICAL_SURFACE ( 'NONE', #1385, 0.1982677165354330695, 0.7853981633974415066 ) ;
#2012 = CYLINDRICAL_SURFACE ( 'NONE', #2815, 0.2362204724409446843 ) ;
#2013 = EDGE_CURVE ( 'NONE', #1170, #7446, #4141, .T. ) ;
#2014 = ORIENTED_EDGE ( 'NONE', *, *, #6907, .F. ) ;
#2015 = B_SPLINE_CURVE_WITH_KNOTS ( 'NONE', 3,
 ( #5849, #2926, #7067, #1828, #3050, #4163 ),
 .UNSPECIFIED., .F., .F.,
 ( 4, 2, 4 ),
 ( 0.004466737480205778058, 0.006712681563759909271, 0.008958625647314040485 ),
 .UNSPECIFIED. ) ;
#2016 = AXIS2_PLACEMENT_3D ( 'NONE', #2371, #5287, #1217 ) ;
#2017 = CARTESIAN_POINT ( 'NONE',  ( -3.198568410424924124, 2.407012729153881203, 0.000000000000000000 ) ) ;
#2018 =( NAMED_UNIT ( * ) PLANE_ANGLE_UNIT ( ) SI_UNIT ( $, .RADIAN. ) );
#2019 = CARTESIAN_POINT ( 'NONE',  ( 0.3426147637089220765, 0.05832033309504411345, -0.3015404986019938893 ) ) ;
#2020 = EDGE_CURVE ( 'NONE', #1140, #1045, #6049, .T. ) ;
#2021 = EDGE_CURVE ( 'NONE', #735, #781, #4255, .T. ) ;
#2022 = ADVANCED_FACE ( 'NONE', ( #1909 ), #7213, .F. ) ;
#2023 = CARTESIAN_POINT ( 'NONE',  ( 0.3336175750056032951, 0.05682581389661665178, 0.2952755905511811885 ) ) ;
#2024 = B_SPLINE_CURVE_WITH_KNOTS ( 'NONE', 3,
 ( #7341, #6778, #5098, #3218, #2120, #3838, #6132, #890 ),
 .UNSPECIFIED., .F., .F.,
 ( 4, 2, 2, 4 ),
 ( 0.004381617662950684777, 0.005472867551409519790, 0.006564117439868355670, 0.008746617216786024829 ),
 .UNSPECIFIED. ) ;
#2025 = DIRECTION ( 'NONE',  ( 1.000000000000000000, 0.000000000000000000, 0.000000000000000000 ) ) ;
#2026 = CARTESIAN_POINT ( 'NONE',  ( 0.3581828924050323715, -0.1743168766271109560, 0.3019256869348722616 ) ) ;
#2027 = CARTESIAN_POINT ( 'NONE',  ( -0.4619485889667617196, 0.9755734897585889298, -1.553989674004691901 ) ) ;
#2028 = ORIENTED_EDGE ( 'NONE', *, *, #2605, .F. ) ;
#2029 = CARTESIAN_POINT ( 'NONE',  ( 5.385555596699504477E-15, -0.5141614760841457521, -2.204724409448820754 ) ) ;
#2030 = B_SPLINE_CURVE_WITH_KNOTS ( 'NONE', 3,
 ( #1912, #2554, #7216, #3824, #4892, #4850, #3094, #840, #2594 ),
 .UNSPECIFIED., .F., .F.,
 ( 4, 2, 1, 2, 4 ),
 ( 0.000000000000000000, 0.002165063509461098799, 0.004330127018922199332, 0.006495190528383298564, 0.008660254037844398664 ),
 .UNSPECIFIED. ) ;
#2031 = DIRECTION ( 'NONE',  ( -1.000000000000000000, 0.000000000000000000, 0.000000000000000000 ) ) ;
#2032 = DIRECTION ( 'NONE',  ( 0.000000000000000000, 0.000000000000000000, 1.000000000000000000 ) ) ;
#2033 = CARTESIAN_POINT ( 'NONE',  ( 0.01165389088406399223, -0.1143408654217484000, -0.2952755905511810219 ) ) ;
#2034 = CARTESIAN_POINT ( 'NONE',  ( 0.4996355910473239681, 1.070877566692228999, -1.498503231159224791 ) ) ;
#2035 = EDGE_LOOP ( 'NONE', ( #253, #4396, #7307, #7352 ) ) ;
#2036 = AXIS2_PLACEMENT_3D ( 'NONE', #6472, #6398, #1728 ) ;
#2037 = CARTESIAN_POINT ( 'NONE',  ( 0.4416272204090973541, -1.010074371201533205, -1.570717485485533249 ) ) ;
#2038 = ORIENTED_EDGE ( 'NONE', *, *, #1441, .F. ) ;
#2039 = PRODUCT_DEFINITION_SHAPE ( 'NONE', 'NONE',  #7521 ) ;
#2040 = ORIENTED_EDGE ( 'NONE', *, *, #983, .F. ) ;
#2041 = CARTESIAN_POINT ( 'NONE',  ( 0.000000000000000000, 0.000000000000000000, -2.204724409448820754 ) ) ;
#2042 = CARTESIAN_POINT ( 'NONE',  ( 0.3432736861146661322, 0.3267484299055463115, 0.02460629921259843353 ) ) ;
#2043 = CARTESIAN_POINT ( 'NONE',  ( -1.041228047528456102, 0.4333661275892043419, -1.574803149606299302 ) ) ;
#2044 = CARTESIAN_POINT ( 'NONE',  ( -5.154746071126634886E-15, 0.4921259842519648542, -2.204724409448822975 ) ) ;
#2045 = VERTEX_POINT ( 'NONE', #5348 ) ;
#2046 = CARTESIAN_POINT ( 'NONE',  ( 0.3336175750056032396, 0.05682581389661631177, -0.2952755905511810219 ) ) ;
#2047 = ORIENTED_EDGE ( 'NONE', *, *, #4027, .T. ) ;
#2048 = CARTESIAN_POINT ( 'NONE',  ( 2.755905511811024056, 1.496062992125984259, 0.000000000000000000 ) ) ;
#2049 = ORIENTED_EDGE ( 'NONE', *, *, #3694, .T. ) ;
#2050 =( LENGTH_UNIT ( ) NAMED_UNIT ( * ) SI_UNIT ( $, .METRE. ) );
#2051 = PRESENTATION_LAYER_ASSIGNMENT (  '', '', ( #2404 ) ) ;
#2052 = CARTESIAN_POINT ( 'NONE',  ( 0.2066929133858267931, 0.000000000000000000, -0.3865922971001068409 ) ) ;
#2053 = ADVANCED_FACE ( 'NONE', ( #2515 ), #6083, .T. ) ;
#2054 = CARTESIAN_POINT ( 'NONE',  ( 1.056523642887397862, 0.5141614760841569653, -1.484898342931014303 ) ) ;
#2055 =( NAMED_UNIT ( * ) SI_UNIT ( $, .STERADIAN. ) SOLID_ANGLE_UNIT ( ) );
#2056 = CARTESIAN_POINT ( 'NONE',  ( -0.9221073153504516506, -0.4437903857718360490, -1.453484209829405849 ) ) ;
#2057 = CIRCLE ( 'NONE', #4007, 1.043121362164705745 ) ;
#2058 = DIRECTION ( 'NONE',  ( -0.000000000000000000, -0.000000000000000000, -1.000000000000000000 ) ) ;
#2059 = EDGE_CURVE ( 'NONE', #6553, #2951, #6008, .T. ) ;
#2060 = EDGE_CURVE ( 'NONE', #428, #3247, #4358, .T. ) ;
#2061 = CARTESIAN_POINT ( 'NONE',  ( 0.3561390657006783811, -0.1723301304999994843, -0.2984845417009731050 ) ) ;
#2062 = AXIS2_PLACEMENT_3D ( 'NONE', #1324, #2485, #4202 ) ;
#2063 = CARTESIAN_POINT ( 'NONE',  ( 0.9752011746067855702, -0.4617902729109746307, -1.554226146212451809 ) ) ;
#2064 = VERTEX_POINT ( 'NONE', #6615 ) ;
#2065 = CARTESIAN_POINT ( 'NONE',  ( -0.9990286922241471412, 0.4596433552321222415, -1.415369843883346412 ) ) ;
#2066 = EDGE_CURVE ( 'NONE', #3143, #4985, #6096, .T. ) ;
#2067 = EDGE_LOOP ( 'NONE', ( #3836, #2637, #1875, #2411 ) ) ;
#2068 = VECTOR ( 'NONE', #5990, 39.37007874015748143 ) ;
#2069 = CARTESIAN_POINT ( 'NONE',  ( -0.1621299108466738859, 0.3155401123846230949, 2.446057743350508180E-16 ) ) ;
#2070 = DIRECTION ( 'NONE',  ( 0.000000000000000000, 0.000000000000000000, 1.000000000000000000 ) ) ;
#2071 = APPLICATION_PROTOCOL_DEFINITION ( 'draft international standard', 'automotive_design', 1998, #2240 ) ;
#2072 = EDGE_CURVE ( 'NONE', #1804, #1607, #2441, .T. ) ;
#2073 = CARTESIAN_POINT ( 'NONE',  ( 0.01832242175888466190, -0.1844213691142429778, -0.2711239997950803393 ) ) ;
#2074 = VERTEX_POINT ( 'NONE', #3167 ) ;
#2075 = DIRECTION ( 'NONE',  ( -0.000000000000000000, -0.000000000000000000, 1.000000000000000000 ) ) ;
#2076 = DIRECTION ( 'NONE',  ( 1.000000000000000000, 0.000000000000000000, 0.000000000000000000 ) ) ;
#2077 = VERTEX_POINT ( 'NONE', #5512 ) ;
#2078 = ORIENTED_EDGE ( 'NONE', *, *, #2987, .F. ) ;
#2079 = LINE ( 'NONE', #6419, #278 ) ;
#2080 = AXIS2_PLACEMENT_3D ( 'NONE', #4998, #4382, #1540 ) ;
#2081 = CARTESIAN_POINT ( 'NONE',  ( 0.9990286721055757768, 0.4596436929058995702, -1.415369458146015447 ) ) ;
#2082 = DIRECTION ( 'NONE',  ( -0.000000000000000000, -1.000000000000000000, -0.000000000000000000 ) ) ;
#2083 = CARTESIAN_POINT ( 'NONE',  ( -9.561467977824920278E-16, -0.4091458600556405756, -0.03164754241312491001 ) ) ;
#2084 = ORIENTED_EDGE ( 'NONE', *, *, #6446, .F. ) ;
#2085 = CARTESIAN_POINT ( 'NONE',  ( 0.9763767025864577009, 0.2362177056199707692, 0.9554858099749828915 ) ) ;
#2086 = ORIENTED_EDGE ( 'NONE', *, *, #1200, .T. ) ;
#2087 = AXIS2_PLACEMENT_3D ( 'NONE', #4032, #6367, #5798 ) ;
#2088 = ORIENTED_EDGE ( 'NONE', *, *, #5445, .T. ) ;
#2089 = VERTEX_POINT ( 'NONE', #2592 ) ;
#2090 = DIRECTION ( 'NONE',  ( -0.5516284119576553291, -0.8340899802305957733, 8.703667695683463275E-16 ) ) ;
#2091 = CARTESIAN_POINT ( 'NONE',  ( 0.000000000000000000, 0.2557161625347749712, -0.1476377952755909551 ) ) ;
#2092 =( REPRESENTATION_RELATIONSHIP ('NONE','NONE', #303, #1307 ) REPRESENTATION_RELATIONSHIP_WITH_TRANSFORMATION ( #2858 )SHAPE_REPRESENTATION_RELATIONSHIP( ) );
#2093 = FACE_BOUND ( 'NONE', #6992, .T. ) ;
#2094 = AXIS2_PLACEMENT_3D ( 'NONE', #2537, #822, #6070 ) ;
#2095 = CARTESIAN_POINT ( 'NONE',  ( 0.4330708661417322913, 1.044891351410287994, -1.574550377471545692 ) ) ;
#2096 = CARTESIAN_POINT ( 'NONE',  ( 0.3336175750056032396, 0.2841290694830835850, -0.09842519685039363697 ) ) ;
#2097 = AXIS2_PLACEMENT_3D ( 'NONE', #2109, #3787, #6120 ) ;
#2098 = DIRECTION ( 'NONE',  ( 0.000000000000000000, -0.5000000000000005551, 0.8660254037844382635 ) ) ;
#2099 = ORIENTED_EDGE ( 'NONE', *, *, #891, .F. ) ;
#2100 = PRODUCT_DEFINITION_SHAPE ( 'NONE', 'NONE',  #7545 ) ;
#2101 = VECTOR ( 'NONE', #1684, 39.37007874015748143 ) ;
#2102 = DIRECTION ( 'NONE',  ( 1.000000000000000000, 0.000000000000000000, -0.000000000000000000 ) ) ;
#2103 = EDGE_CURVE ( 'NONE', #7275, #7079, #1184, .T. ) ;
#2104 = SHAPE_REPRESENTATION ( 'MAT-019 Puller', ( #5166 ), #7344 ) ;
#2105 = AXIS2_PLACEMENT_3D ( 'NONE', #5800, #5257, #5869 ) ;
#2106 = VERTEX_POINT ( 'NONE', #3086 ) ;
#2107 = CIRCLE ( 'NONE', #3934, 0.2362204724409449064 ) ;
#2108 = CARTESIAN_POINT ( 'NONE',  ( 0.01168997831664858947, 0.1984671517595417711, 0.2467959906213527677 ) ) ;
#2109 = CARTESIAN_POINT ( 'NONE',  ( 0.000000000000000000, 0.000000000000000000, -2.204724409448820754 ) ) ;
#2110 = AXIS2_PLACEMENT_3D ( 'NONE', #4031, #5796, #555 ) ;
#2111 = DIRECTION ( 'NONE',  ( 0.000000000000000000, 0.000000000000000000, 1.000000000000000000 ) ) ;
#2112 = CONTEXT_DEPENDENT_SHAPE_REPRESENTATION ( #7204, #6554 ) ;
#2113 = CARTESIAN_POINT ( 'NONE',  ( -0.4342018836190598141, -0.9783380834473016652, -1.450123305573145283 ) ) ;
#2114 = VERTEX_POINT ( 'NONE', #3706 ) ;
#2115 = CIRCLE ( 'NONE', #5170, 0.2362204724409449619 ) ;
#2116 = EDGE_CURVE ( 'NONE', #3650, #6826, #6159, .T. ) ;
#2117 = EDGE_CURVE ( 'NONE', #2154, #3264, #6573, .T. ) ;
#2118 = ORIENTED_EDGE ( 'NONE', *, *, #3754, .T. ) ;
#2119 = VERTEX_POINT ( 'NONE', #795 ) ;
#2120 = CARTESIAN_POINT ( 'NONE',  ( 0.004822332172886453772, -0.2917300191221102734, -0.08525996588982823199 ) ) ;
#2121 = LENGTH_MEASURE_WITH_UNIT ( LENGTH_MEASURE( 0.02539999999999999897 ), #3727 );
#2122 = EDGE_LOOP ( 'NONE', ( #2794, #5563, #5711 ) ) ;
#2123 = CARTESIAN_POINT ( 'NONE',  ( 0.3411151615605803600, 0.2304996462388439749, 0.2037536041052391000 ) ) ;
#2124 = VERTEX_POINT ( 'NONE', #5965 ) ;
#2125 = CARTESIAN_POINT ( 'NONE',  ( 0.3432736861146659657, 0.1420645347415414039, -0.2952755905511810219 ) ) ;
#2126 = EDGE_LOOP ( 'NONE', ( #860, #5073, #328 ) ) ;
#2127 = ORIENTED_EDGE ( 'NONE', *, *, #2978, .F. ) ;
#2128 = CARTESIAN_POINT ( 'NONE',  ( 0.3426022948973417304, -0.05819196463765255456, -0.3015401604570891458 ) ) ;
#2129 = DIRECTION ( 'NONE',  ( -0.04025208698423568543, -0.9991895563372417133, 5.172723957598567426E-16 ) ) ;
#2130 = CARTESIAN_POINT ( 'NONE',  ( 1.279527559055118280, 1.968503937007874072, 2.480314960629921295 ) ) ;
#2131 = DIRECTION ( 'NONE',  ( 1.000000000000000000, 0.000000000000000000, 0.000000000000000000 ) ) ;
#2132 = PRESENTATION_STYLE_ASSIGNMENT (( #4880 ) ) ;
#2133 = CYLINDRICAL_SURFACE ( 'NONE', #4313, 0.2362204724409448231 ) ;
#2134 = DIRECTION ( 'NONE',  ( 0.000000000000000000, 0.000000000000000000, 1.000000000000000000 ) ) ;
#2135 = DIRECTION ( 'NONE',  ( -0.000000000000000000, -1.000000000000000000, -0.000000000000000000 ) ) ;
#2136 = PLANE ( 'NONE',  #4877 ) ;
#2137 = CARTESIAN_POINT ( 'NONE',  ( -1.279527559055118280, 1.968503937007874072, 0.4724409448818898127 ) ) ;
#2138 = CARTESIAN_POINT ( 'NONE',  ( -1.126887297386508504E-15, -0.4091458600556405756, -0.3766201741223081378 ) ) ;
#2139 = EDGE_LOOP ( 'NONE', ( #6526, #5681, #1655, #521, #7071, #2334, #1519 ) ) ;
#2140 = CARTESIAN_POINT ( 'NONE',  ( 0.000000000000000000, 1.496062992125984259, 0.4921259842519685179 ) ) ;
#2141 = CARTESIAN_POINT ( 'NONE',  ( 0.9666437042230172638, -0.4330708661417221883, -1.454455828411335583 ) ) ;
#2142 = B_SPLINE_CURVE_WITH_KNOTS ( 'NONE', 3,
 ( #4967, #2591, #837, #7324, #3858, #985, #1431, #950, #6722, #3781 ),
 .UNSPECIFIED., .F., .F.,
 ( 4, 2, 2, 2, 4 ),
 ( 3.469446951953614189E-18, 0.0005494620090385992067, 0.001098924018077194944, 0.001648386027115790681, 0.002197848036154386418 ),
 .UNSPECIFIED. ) ;
#2143 = CARTESIAN_POINT ( 'NONE',  ( 0.3391892065151631552, -0.1988903486381589925, -0.2460629921259842035 ) ) ;
#2144 = VERTEX_POINT ( 'NONE', #227 ) ;
#2145 = CARTESIAN_POINT ( 'NONE',  ( 0.3585569128062319200, 0.3496569568119790028, 0.001755940978325809575 ) ) ;
#2146 = CARTESIAN_POINT ( 'NONE',  ( -1.056523642887404968, 0.5141614760841421994, -1.484898342931014525 ) ) ;
#2147 = SHAPE_REPRESENTATION ( 'Bolt', ( #5166 ), #3072 ) ;
#2148 = EDGE_LOOP ( 'NONE', ( #1753, #6361 ) ) ;
#2149 = ORIENTED_EDGE ( 'NONE', *, *, #2522, .F. ) ;
#2150 = DIRECTION ( 'NONE',  ( 0.000000000000000000, 0.000000000000000000, 1.000000000000000000 ) ) ;
#2151 = CARTESIAN_POINT ( 'NONE',  ( 0.3410425348215775920, 0.2462961272004790259, 0.1763890642357578975 ) ) ;
#2152 = ADVANCED_FACE ( 'NONE', ( #3120 ), #5119, .T. ) ;
#2153 = CARTESIAN_POINT ( 'NONE',  ( 0.01832242175888482497, -0.3270109559553083245, 0.02415159075610082487 ) ) ;
#2154 = VERTEX_POINT ( 'NONE', #3045 ) ;
#2155 = EDGE_CURVE ( 'NONE', #489, #5247, #2394, .T. ) ;
#2156 = CARTESIAN_POINT ( 'NONE',  ( 2.892866454678787531E-17, 1.496062992125984259, 0.2362204724409449341 ) ) ;
#2157 = ORIENTED_EDGE ( 'NONE', *, *, #5684, .T. ) ;
#2158 = CARTESIAN_POINT ( 'NONE',  ( -0.4330708661417317362, 1.048552902599920733, -1.573978973432617279 ) ) ;
#2159 = ORIENTED_EDGE ( 'NONE', *, *, #7058, .T. ) ;
#2160 = CARTESIAN_POINT ( 'NONE',  ( 0.3487102105009254327, 0.3201373431253348167, 0.04891434758976444946 ) ) ;
#2161 = EDGE_CURVE ( 'NONE', #1045, #7070, #2787, .T. ) ;
#2162 = CARTESIAN_POINT ( 'NONE',  ( 0.000000000000000000, 0.000000000000000000, -0.2952755905511810774 ) ) ;
#2163 = VERTEX_POINT ( 'NONE', #4317 ) ;
#2164 = CARTESIAN_POINT ( 'NONE',  ( -0.9346850374427957409, 0.4388996395293537911, -1.455943645409046638 ) ) ;
#2165 = CARTESIAN_POINT ( 'NONE',  ( 18.30767084476530826, 38.73487850451991221, 51.90956403617312276 ) ) ;
#2166 = CARTESIAN_POINT ( 'NONE',  ( 0.3505601438611540277, -0.1704774416898505729, -0.2952755905511810774 ) ) ;
#2167 = DIRECTION ( 'NONE',  ( 0.000000000000000000, 0.000000000000000000, 1.000000000000000000 ) ) ;
#2168 = ADVANCED_FACE ( 'NONE', ( #721 ), #6650, .T. ) ;
#2169 = DIRECTION ( 'NONE',  ( 1.000000000000000000, 0.000000000000000000, -0.000000000000000000 ) ) ;
#2170 = VECTOR ( 'NONE', #5143, 39.37007874015748143 ) ;
#2171 = SHAPE_REPRESENTATION_RELATIONSHIP ( 'NONE' , 'NONE' ,  #785, #5957 ) ;
#2172 = CARTESIAN_POINT ( 'NONE',  ( 0.4437902010346556625, 0.9221077491748230770, -1.453484313640521552 ) ) ;
#2173 = CARTESIAN_POINT ( 'NONE',  ( 0.3388536909602617997, -0.2864058322153867353, 0.09448172812127884901 ) ) ;
#2174 = CARTESIAN_POINT ( 'NONE',  ( 0.000000000000000000, 0.2557161625347750267, 0.1476377952755908163 ) ) ;
#2175 = AXIS2_PLACEMENT_3D ( 'NONE', #2590, #871, #1430 ) ;
#2176 = DIRECTION ( 'NONE',  ( 0.000000000000000000, 0.000000000000000000, -1.000000000000000000 ) ) ;
#2177 = ORIENTED_EDGE ( 'NONE', *, *, #7461, .T. ) ;
#2178 = CARTESIAN_POINT ( 'NONE',  ( 0.4406689276647596243, -0.9921522615226822106, -1.439080857166193939 ) ) ;
#2179 = CARTESIAN_POINT ( 'NONE',  ( 1.850393700787401619, 0.7480314960629921295, -0.7480314960629921295 ) ) ;
#2180 = ITEM_DEFINED_TRANSFORMATION ( 'NONE', 'NONE', #2463,  #5166 ) ;
#2181 = CARTESIAN_POINT ( 'NONE',  ( -0.5141614760841421994, 0.000000000000000000, -2.204724409448823419 ) ) ;
#2182 = ORIENTED_EDGE ( 'NONE', *, *, #298, .T. ) ;
#2184 = CARTESIAN_POINT ( 'NONE',  ( 0.3465694189146783510, 0.1966695024996976682, -0.2499096104736449331 ) ) ;
#2183 = DIMENSIONAL_EXPONENTS ( 1.000000000000000000, 0.000000000000000000, 0.000000000000000000, 0.000000000000000000, 0.000000000000000000, 0.000000000000000000, 0.000000000000000000 ) ;
#2185 = CARTESIAN_POINT ( 'NONE',  ( 0.3465694189147059956, -0.1966695024996656382, 0.2499096104736426016 ) ) ;
#2186 = CIRCLE ( 'NONE', #3158, 0.2952755905511810774 ) ;
#2187 = ORIENTED_EDGE ( 'NONE', *, *, #5635, .T. ) ;
#2188 = ORIENTED_EDGE ( 'NONE', *, *, #7005, .F. ) ;
#2189 = CARTESIAN_POINT ( 'NONE',  ( 0.2948818897637794367, 0.000000000000000000, 0.1188976377952756375 ) ) ;
#2190 = CARTESIAN_POINT ( 'NONE',  ( 0.3425764178929368575, 0.2900721174007582781, 0.1006592143205869566 ) ) ;
#2191 = AXIS2_PLACEMENT_3D ( 'NONE', #5007, #4392, #2628 ) ;
#2192 = ORIENTED_EDGE ( 'NONE', *, *, #7183, .T. ) ;
#2193 = CARTESIAN_POINT ( 'NONE',  ( 0.0006233585804807679088, 0.2412158484082065346, -0.1727530760685158651 ) ) ;
#2194 = ORIENTED_EDGE ( 'NONE', *, *, #5577, .F. ) ;
#2195 = CARTESIAN_POINT ( 'NONE',  ( 1.171887040486664588, 0.1443386382778019672, 0.9736977440596933375 ) ) ;
#2196 = CARTESIAN_POINT ( 'NONE',  ( 0.3388536909603142577, 0.2250264928541962084, 0.2007938624298919450 ) ) ;
#2197 = EDGE_LOOP ( 'NONE', ( #4632, #5501, #2049, #2996 ) ) ;
#2198 = AXIS2_PLACEMENT_3D ( 'NONE', #5282, #4790, #1921 ) ;
#2199 = EDGE_CURVE ( 'NONE', #3405, #3650, #4011, .T. ) ;
#2200 = ORIENTED_EDGE ( 'NONE', *, *, #6928, .T. ) ;
#2201 = DIRECTION ( 'NONE',  ( -1.000000000000000000, -0.000000000000000000, -0.000000000000000000 ) ) ;
#2202 = DIRECTION ( 'NONE',  ( -2.251170071535831168E-15, 6.436324498194447478E-16, 1.000000000000000000 ) ) ;
#2203 = DIRECTION ( 'NONE',  ( 1.000000000000000000, 0.000000000000000000, 2.207829878515936732E-15 ) ) ;
#2204 = TOROIDAL_SURFACE ( 'NONE', #501, 0.4507874015748032370, 0.03543307086614166934 ) ;
#2205 = CARTESIAN_POINT ( 'NONE',  ( 0.000000000000000000, 0.000000000000000000, 0.000000000000000000 ) ) ;
#2206 = CARTESIAN_POINT ( 'NONE',  ( 1.162092266633492077, 0.1562322077656922159, -0.9718357064180906946 ) ) ;
#2207 = EDGE_CURVE ( 'NONE', #3331, #4739, #2992, .T. ) ;
#2208 = EDGE_CURVE ( 'NONE', #4818, #1261, #4624, .T. ) ;
#2209 = CARTESIAN_POINT ( 'NONE',  ( 0.000000000000000000, 0.000000000000000000, -0.8561751947315059397 ) ) ;
#2210 = LINE ( 'NONE', #3933, #7365 ) ;
#2211 = CARTESIAN_POINT ( 'NONE',  ( 0.3391216574608478806, -0.3159523085418498023, 0.04330572993920116937 ) ) ;
#2212 = DIRECTION ( 'NONE',  ( 1.000000000000000000, 0.000000000000000000, 0.000000000000000000 ) ) ;
#2213 = B_SPLINE_CURVE_WITH_KNOTS ( 'NONE', 3,
 ( #143, #4806, #7132, #7166, #1899, #4230, #3660, #5425, #4423, #6074, #7203, #2697, #6795, #3850, #260, #1978, #978, #6714, #414, #1541, #828, #4383, #2583, #7357, #6183, #6149, #1391, #6108, #5582, #4921, #1459, #7278, #7247, #3268, #6752, #5620, #6642, #3197, #3889, #4346 ),
 .UNSPECIFIED., .F., .F.,
 ( 4, 2, 2, 2, 2, 2, 2, 2, 2, 2, 2, 2, 2, 2, 2, 2, 2, 2, 2, 4 ),
 ( 0.01882766236946021784, 0.02000407617178198011, 0.02118048997410373890, 0.02176869687526461830, 0.02235690377642549770, 0.02353331757874724955, 0.02470973138106900141, 0.02588614518339075327, 0.02706255898571250512, 0.02765076588687337758, 0.02823897278803425004, 0.02941538659035599496, 0.03059180039267773293, 0.03176821419499947785, 0.03235642109616034684, 0.03294462799732121583, 0.03412104179964296768, 0.03529745560196471260, 0.03647386940428645752, 0.03765028320660820244 ),
 .UNSPECIFIED. ) ;
#2214 = VERTEX_POINT ( 'NONE', #6028 ) ;
#2215 = AXIS2_PLACEMENT_3D ( 'NONE', #5072, #2892, #7273 ) ;
#2216 = CARTESIAN_POINT ( 'NONE',  ( -1.279527559055117836, 1.968503937007873850, 0.000000000000000000 ) ) ;
#2217 = VERTEX_POINT ( 'NONE', #7043 ) ;
#2218 = CARTESIAN_POINT ( 'NONE',  ( 0.000000000000000000, 0.000000000000000000, -3.582716535433073002 ) ) ;
#2219 = DIRECTION ( 'NONE',  ( -0.000000000000000000, -0.000000000000000000, 1.000000000000000000 ) ) ;
#2220 = CIRCLE ( 'NONE', #5035, 0.4507874015748032370 ) ;
#2221 = FACE_OUTER_BOUND ( 'NONE', #2563, .T. ) ;
#2222 = VERTEX_POINT ( 'NONE', #6523 ) ;
#2223 = CARTESIAN_POINT ( 'NONE',  ( 0.3496875272944827695, 0.1667004943313749321, -0.3018174552735724547 ) ) ;
#2224 = CARTESIAN_POINT ( 'NONE',  ( 0.3565325103478088065, -0.3440765519545064266, -0.005406888575953978406 ) ) ;
#2225 = AXIS2_PLACEMENT_3D ( 'NONE', #5000, #2739, #1586 ) ;
#2226 = CIRCLE ( 'NONE', #5407, 0.2362204724409449064 ) ;
#2227 = VECTOR ( 'NONE', #806, 39.37007874015748143 ) ;
#2228 = VERTEX_POINT ( 'NONE', #1800 ) ;
#2229 = CARTESIAN_POINT ( 'NONE',  ( 1.102718734937994105, -0.2049554913489460561, 0.9627163727494573164 ) ) ;
#2230 = CARTESIAN_POINT ( 'NONE',  ( -0.4339190921229451603, 0.9541934910893049571, -1.456692913385828847 ) ) ;
#2231 = AXIS2_PLACEMENT_3D ( 'NONE', #5196, #4006, #1736 ) ;
#2232 = CARTESIAN_POINT ( 'NONE',  ( 1.089828288828796898, -1.334654725534422735E-16, -1.361499588670820771 ) ) ;
#2233 = ORIENTED_EDGE ( 'NONE', *, *, #5280, .T. ) ;
#2234 = CARTESIAN_POINT ( 'NONE',  ( 0.01171324505787542034, 0.1984117137466533121, -0.2468920120763460069 ) ) ;
#2235 = EDGE_LOOP ( 'NONE', ( #1750, #3381, #3394, #5682 ) ) ;
#2236 = CARTESIAN_POINT ( 'NONE',  ( 2.892866454678787531E-17, 0.2559055118110236116, 0.2362204724409449341 ) ) ;
#2237 = EDGE_LOOP ( 'NONE', ( #2579, #6388, #6195, #6601 ) ) ;
#2238 = CIRCLE ( 'NONE', #1992, 0.2699662542182227343 ) ;
#2239 = DIMENSIONAL_EXPONENTS ( 1.000000000000000000, 0.000000000000000000, 0.000000000000000000, 0.000000000000000000, 0.000000000000000000, 0.000000000000000000, 0.000000000000000000 ) ;
#2240 = APPLICATION_CONTEXT ( 'automotive_design' ) ;
#2241 = CARTESIAN_POINT ( 'NONE',  ( 7.874015748031496287, 0.2559055118110236116, -0.2362204724409455170 ) ) ;
#2242 = CARTESIAN_POINT ( 'NONE',  ( 25.13671773485890526, 34.81515369617522992, 55.32688687081880374 ) ) ;
#2243 = DIRECTION ( 'NONE',  ( -1.000000000000000000, -0.000000000000000000, -0.000000000000000000 ) ) ;
#2244 = CARTESIAN_POINT ( 'NONE',  ( -0.9666437042230129340, -0.4330708661417356220, -1.454455828411337359 ) ) ;
#2245 = VECTOR ( 'NONE', #1273, 39.37007874015748143 ) ;
#2246 = EDGE_CURVE ( 'NONE', #3292, #6423, #1304, .T. ) ;
#2247 = DIRECTION ( 'NONE',  ( 0.000000000000000000, -0.000000000000000000, 1.000000000000000000 ) ) ;
#2248 = CARTESIAN_POINT ( 'NONE',  ( 0.3581828924050324825, 0.3486337532542225226, 1.056976728655274672E-17 ) ) ;
#2249 = CYLINDRICAL_SURFACE ( 'NONE', #3466, 1.968503937007874072 ) ;
#2250 = EDGE_CURVE ( 'NONE', #1132, #6852, #1266, .T. ) ;
#2251 = DIRECTION ( 'NONE',  ( -4.625929269271482167E-15, 0.000000000000000000, 1.000000000000000000 ) ) ;
#2252 = EDGE_CURVE ( 'NONE', #3756, #1492, #6792, .T. ) ;
#2253 = DIRECTION ( 'NONE',  ( -1.000000000000000000, 0.000000000000000000, -2.193342766891361226E-15 ) ) ;
#2254 = AXIS2_PLACEMENT_3D ( 'NONE', #6692, #4974, #6726 ) ;
#2255 = EDGE_CURVE ( 'NONE', #3901, #3073, #582, .T. ) ;
#2256 = CARTESIAN_POINT ( 'NONE',  ( 0.3306743754077733910, -1.707404996040164512E-17, 0.2952755905511811885 ) ) ;
#2257 = FACE_OUTER_BOUND ( 'NONE', #6587, .T. ) ;
#2258 = CARTESIAN_POINT ( 'NONE',  ( -0.9867938558989102216, -0.4882975260543767071, -1.385219839936553177 ) ) ;
#2259 = ORIENTED_EDGE ( 'NONE', *, *, #1119, .F. ) ;
#2260 = CARTESIAN_POINT ( 'NONE',  ( 0.3531511627980760681, 0.1878266560944092389, -0.2783075040405467715 ) ) ;
#2261 = DIRECTION ( 'NONE',  ( 1.000000000000000000, 0.000000000000000000, 0.000000000000000000 ) ) ;
#2262 = ORIENTED_EDGE ( 'NONE', *, *, #6405, .F. ) ;
#2263 = CARTESIAN_POINT ( 'NONE',  ( 1.220472440944881942, -0.01566924555314537157, 0.9842519685039372579 ) ) ;
#2264 = LENGTH_MEASURE_WITH_UNIT ( LENGTH_MEASURE( 0.02539999999999999897 ), #5688 );
#2265 = CARTESIAN_POINT ( 'NONE',  ( 0.3391892065151631552, -0.3125419764313924209, 0.04921259842519686012 ) ) ;
#2266 = VERTEX_POINT ( 'NONE', #7372 ) ;
#2267 = CARTESIAN_POINT ( 'NONE',  ( 0.9666437042230099363, 0.4330708661417423944, -1.454455828411337359 ) ) ;
#2268 = CARTESIAN_POINT ( 'NONE',  ( 0.3410249605999032263, -0.02920150297965336608, 0.3014927230551895931 ) ) ;
#2269 = ORIENTED_EDGE ( 'NONE', *, *, #145, .T. ) ;
#2270 = FACE_OUTER_BOUND ( 'NONE', #5207, .T. ) ;
#2271 = DIRECTION ( 'NONE',  ( -0.000000000000000000, -0.000000000000000000, -1.000000000000000000 ) ) ;
#2272 = CARTESIAN_POINT ( 'NONE',  ( -0.05806029764938282212, 0.3756247315785394836, -0.3942118233966397933 ) ) ;
#2273 = PRODUCT_DEFINITION_FORMATION_WITH_SPECIFIED_SOURCE ( 'ANY', '', #6010, .NOT_KNOWN. ) ;
#2274 = CARTESIAN_POINT ( 'NONE',  ( 0.3391892065151630442, 0.3125419764313920878, -0.04921259842519681155 ) ) ;
#2275 = EDGE_CURVE ( 'NONE', #614, #3721, #598, .T. ) ;
#2276 = DIRECTION ( 'NONE',  ( 1.000000000000000000, 0.000000000000000000, 0.000000000000000000 ) ) ;
#2277 = DIRECTION ( 'NONE',  ( 0.000000000000000000, 0.000000000000000000, -1.000000000000000000 ) ) ;
#2278 = LINE ( 'NONE', #4193, #2599 ) ;
#2279 = CARTESIAN_POINT ( 'NONE',  ( 0.3391892065151629332, -0.1136516277932332758, 0.2952755905511811885 ) ) ;
#2280 = ADVANCED_FACE ( 'NONE', ( #5747 ), #961, .F. ) ;
#2281 = ADVANCED_FACE ( 'NONE', ( #4015 ), #815, .F. ) ;
#2282 = DIRECTION ( 'NONE',  ( -1.000000000000000000, 0.000000000000000000, 0.000000000000000000 ) ) ;
#2283 = ITEM_DEFINED_TRANSFORMATION ( 'NONE', 'NONE', #4231,  #5166 ) ;
#2284 = VECTOR ( 'NONE', #3018, 39.37007874015748143 ) ;
#2285 = EDGE_CURVE ( 'NONE', #345, #7028, #243, .T. ) ;
#2286 = CARTESIAN_POINT ( 'NONE',  ( -0.4999740374263542675, -0.9773781006402580962, -1.373989084484001477 ) ) ;
#2287 = B_SPLINE_CURVE_WITH_KNOTS ( 'NONE', 3,
 ( #6766, #277, #2558, #2598 ),
 .UNSPECIFIED., .F., .F.,
 ( 4, 4 ),
 ( 6.938893903907228378E-18, 0.0002807012396509452013 ),
 .UNSPECIFIED. ) ;
#2288 = ORIENTED_EDGE ( 'NONE', *, *, #2769, .T. ) ;
#2289 = FACE_OUTER_BOUND ( 'NONE', #6723, .T. ) ;
#2290 = VERTEX_POINT ( 'NONE', #1644 ) ;
#2291 = VECTOR ( 'NONE', #5435, 39.37007874015748143 ) ;
#2292 = EDGE_CURVE ( 'NONE', #5027, #448, #4384, .T. ) ;
#2293 = ORIENTED_EDGE ( 'NONE', *, *, #5445, .F. ) ;
#2294 = EDGE_CURVE ( 'NONE', #5092, #7286, #3382, .T. ) ;
#2295 = CARTESIAN_POINT ( 'NONE',  ( -0.1771653543307089573, 0.3068593950417301541, 0.000000000000000000 ) ) ;
#2296 = DIRECTION ( 'NONE',  ( -0.000000000000000000, -0.000000000000000000, 1.000000000000000000 ) ) ;
#2297 = EDGE_LOOP ( 'NONE', ( #4287, #550, #1632 ) ) ;
#2298 = AXIS2_PLACEMENT_3D ( 'NONE', #88, #7007, #4797 ) ;
#2299 = FACE_OUTER_BOUND ( 'NONE', #3723, .T. ) ;
#2300 = DIRECTION ( 'NONE',  ( 0.5000000000000006661, -0.8660254037844382635, 0.000000000000000000 ) ) ;
#2301 = ORIENTED_EDGE ( 'NONE', *, *, #6878, .T. ) ;
#2302 = EDGE_LOOP ( 'NONE', ( #182, #3445 ) ) ;
#2303 = DIRECTION ( 'NONE',  ( 0.000000000000000000, 0.5000000000000018874, 0.8660254037844375974 ) ) ;
#2304 = CIRCLE ( 'NONE', #6585, 0.2362204724409448231 ) ;
#2305 = DIRECTION ( 'NONE',  ( 0.000000000000000000, 0.000000000000000000, 1.000000000000000000 ) ) ;
#2306 = CARTESIAN_POINT ( 'NONE',  ( 0.9221077491748198574, 0.4437902010346655435, -1.453484313640523107 ) ) ;
#2307 = FACE_OUTER_BOUND ( 'NONE', #5911, .T. ) ;
#2308 = CIRCLE ( 'NONE', #6234, 0.4629062255509093782 ) ;
#2309 = DIRECTION ( 'NONE',  ( -0.000000000000000000, 0.000000000000000000, 1.000000000000000000 ) ) ;
#2310 = CARTESIAN_POINT ( 'NONE',  ( 2.755905511811024056, 1.496062992125984259, 0.2362204724409449896 ) ) ;
#2311 = CARTESIAN_POINT ( 'NONE',  ( 1.220472440944881942, 0.7480314960629921295, 0.000000000000000000 ) ) ;
#2312 = FACE_OUTER_BOUND ( 'NONE', #3182, .T. ) ;
#2313 = CARTESIAN_POINT ( 'NONE',  ( 0.3432736861146659657, -0.1420645347415416260, 0.2952755905511810774 ) ) ;
#2314 = CARTESIAN_POINT ( 'NONE',  ( 0.3483227611829848303, 0.3409548833797004797, 0.000000000000000000 ) ) ;
#2315 = CONTEXT_DEPENDENT_SHAPE_REPRESENTATION ( #29, #812 ) ;
#2316 = AXIS2_PLACEMENT_3D ( 'NONE', #6416, #1874, #4695 ) ;
#2317 = CARTESIAN_POINT ( 'NONE',  ( 0.3561392902752972267, -0.1723302545757742776, 0.2984847566065203517 ) ) ;
#2318 = ORIENTED_EDGE ( 'NONE', *, *, #6794, .F. ) ;
#2319 = CARTESIAN_POINT ( 'NONE',  ( -0.4508656291625802726, -1.083410641227605886, -1.549345754620972349 ) ) ;
#2320 = EDGE_CURVE ( 'NONE', #6033, #4139, #5641, .T. ) ;
#2321 = CARTESIAN_POINT ( 'NONE',  ( 0.3410076799406686066, -0.2467857494855110190, 0.1755389823809323790 ) ) ;
#2322 = ORIENTED_EDGE ( 'NONE', *, *, #3893, .F. ) ;
#2323 = CIRCLE ( 'NONE', #2456, 1.168853328413307358 ) ;
#2324 = ORIENTED_EDGE ( 'NONE', *, *, #4164, .T. ) ;
#2325 = FACE_OUTER_BOUND ( 'NONE', #1282, .T. ) ;
#2326 = CARTESIAN_POINT ( 'NONE',  ( 3.027559055118110187, 0.000000000000000000, 0.000000000000000000 ) ) ;
#2327 = VERTEX_POINT ( 'NONE', #6383 ) ;
#2328 = AXIS2_PLACEMENT_3D ( 'NONE', #5729, #3884, #976 ) ;
#2329 = CARTESIAN_POINT ( 'NONE',  ( -1.866451592287363150E-29, 1.781909941321919274E-15, -1.397637795275591843 ) ) ;
#2330 = EDGE_CURVE ( 'NONE', #6852, #5590, #4050, .T. ) ;
#2331 = ADVANCED_FACE ( 'NONE', ( #3356 ), #1900, .F. ) ;
#2332 = AXIS2_PLACEMENT_3D ( 'NONE', #1960, #6631, #4291 ) ;
#2333 = CARTESIAN_POINT ( 'NONE',  ( -1.030265555772312824, 0.4349482935633047220, -1.574803149606299302 ) ) ;
#2334 = ORIENTED_EDGE ( 'NONE', *, *, #4305, .T. ) ;
#2335 =( BOUNDED_SURFACE ( )  B_SPLINE_SURFACE ( 3, 2, ( 
 ( #1957, #921, #4445 ),
 ( #773, #3100, #5448 ),
 ( #207, #6628, #2528 ),
 ( #1376, #3722, #810 ),
 ( #3140, #1408, #4899 ),
 ( #4331, #3757, #3178 ),
 ( #6849, #3951, #4594 ),
 ( #6809, #7373, #5137 ) ),
 .UNSPECIFIED., .F., .F., .F. ) 
 B_SPLINE_SURFACE_WITH_KNOTS ( ( 4, 2, 2, 4 ),
 ( 3, 3 ),
 ( 0.03551798592901333346, 0.03994769179990642627, 0.04216254473535296921, 0.04437739767079951908 ),
 ( 0.000000000000000000, 1.000000000000000000 ),
 .UNSPECIFIED. ) 
 GEOMETRIC_REPRESENTATION_ITEM ( )  RATIONAL_B_SPLINE_SURFACE ( (
 ( 1.000000000000000000, 0.8047781103519390244, 1.000000000000000000),
 ( 1.000000000000000000, 0.8123785826175446978, 1.000000000000000000),
 ( 1.000000000000000000, 0.8190671539027887249, 1.000000000000000000),
 ( 1.000000000000000000, 0.8191932076453414258, 1.000000000000000000),
 ( 1.000000000000000000, 0.8176085094066379844, 1.000000000000000000),
 ( 1.000000000000000000, 0.8122955484014008354, 1.000000000000000000),
 ( 1.000000000000000000, 0.8086308001280824165, 1.000000000000000000),
 ( 1.000000000000000000, 0.8047712537969731184, 1.000000000000000000) ) ) 
 REPRESENTATION_ITEM ( '' )  SURFACE ( )  );
#2336 = COLOUR_RGB ( '',0.7921568627450980005, 0.8196078431372548767, 0.9333333333333333481 ) ;
#2337 = AXIS2_PLACEMENT_3D ( 'NONE', #1835, #4249, #3639 ) ;
#2338 = FACE_OUTER_BOUND ( 'NONE', #1369, .T. ) ;
#2339 = LINE ( 'NONE', #2945, #2638 ) ;
#2340 = CARTESIAN_POINT ( 'NONE',  ( 0.000000000000000000, -0.2557161625347748601, 0.1476377952755911216 ) ) ;
#2341 = CARTESIAN_POINT ( 'NONE',  ( 0.3391221370943153790, -0.1204748818123362597, 0.2952755905511811330 ) ) ;
#2342 = ORIENTED_EDGE ( 'NONE', *, *, #4867, .T. ) ;
#2343 = AXIS2_PLACEMENT_3D ( 'NONE', #1445, #5599, #886 ) ;
#2344 = CARTESIAN_POINT ( 'NONE',  ( 0.3483227611829848303, 0.3409548833797004797, 0.000000000000000000 ) ) ;
#2345 = CARTESIAN_POINT ( 'NONE',  ( 0.7480314960629921295, 0.007724973897226917324, -0.9842519685039369248 ) ) ;
#2346 = EDGE_LOOP ( 'NONE', ( #391, #7371, #3826, #576, #3602, #248 ) ) ;
#2347 = CONICAL_SURFACE ( 'NONE', #6637, 0.2952755905511810774, 1.047197551196600518 ) ;
#2348 = CARTESIAN_POINT ( 'NONE',  ( 0.3565422270302660013, -0.3441025489056189213, 0.005451916616122784963 ) ) ;
#2349 = CARTESIAN_POINT ( 'NONE',  ( -0.3543307086614173596, 0.03458999977076007704, 3.331440607508054140E-17 ) ) ;
#2350 = DIRECTION ( 'NONE',  ( 0.000000000000000000, 1.000000000000000000, 2.193342766891360832E-15 ) ) ;
#2351 = CARTESIAN_POINT ( 'NONE',  ( 0.3565325281581928074, 0.1767208741530144900, -0.2952755905511811330 ) ) ;
#2352 = CARTESIAN_POINT ( 'NONE',  ( -0.4541662050560832387, -0.9857970000181586201, -1.560880783937515170 ) ) ;
#2353 = CARTESIAN_POINT ( 'NONE',  ( 0.9666437042230099363, 0.4330708661417423944, -1.454455828411337359 ) ) ;
#2354 = CARTESIAN_POINT ( 'NONE',  ( 0.000000000000000000, 0.000000000000000000, 0.000000000000000000 ) ) ;
#2355 = DIRECTION ( 'NONE',  ( -2.312579046053608732E-29, 2.207829878515936732E-15, 1.000000000000000000 ) ) ;
#2356 = ORIENTED_EDGE ( 'NONE', *, *, #1670, .F. ) ;
#2357 = VECTOR ( 'NONE', #5697, 39.37007874015748143 ) ;
#2358 = CARTESIAN_POINT ( 'NONE',  ( -0.4403524516313984116, -1.075169953371343023, -1.561970681382796045 ) ) ;
#2359 = CARTESIAN_POINT ( 'NONE',  ( 1.968503937007874072, 0.000000000000000000, 0.000000000000000000 ) ) ;
#2360 = ORIENTED_EDGE ( 'NONE', *, *, #6264, .T. ) ;
#2361 = ORIENTED_EDGE ( 'NONE', *, *, #4918, .F. ) ;
#2362 = AXIS2_PLACEMENT_3D ( 'NONE', #451, #6043, #4314 ) ;
#2363 = CARTESIAN_POINT ( 'NONE',  ( 0.8658672433185115036, -0.2045602151624222043, 0.9627673662903735163 ) ) ;
#2364 = EDGE_CURVE ( 'NONE', #1068, #5707, #6877, .T. ) ;
#2365 =( REPRESENTATION_RELATIONSHIP ('NONE','NONE', #303, #5265 ) REPRESENTATION_RELATIONSHIP_WITH_TRANSFORMATION ( #5882 )SHAPE_REPRESENTATION_RELATIONSHIP( ) );
#2366 = DIRECTION ( 'NONE',  ( 0.000000000000000000, 0.000000000000000000, -1.000000000000000000 ) ) ;
#2367 = VERTEX_POINT ( 'NONE', #1508 ) ;
#2368 = PLANE ( 'NONE',  #3082 ) ;
#2369 = LINE ( 'NONE', #6467, #1328 ) ;
#2370 = EDGE_LOOP ( 'NONE', ( #1267, #2028 ) ) ;
#2371 = CARTESIAN_POINT ( 'NONE',  ( 0.9842519685039370358, 0.7480314960629921295, 0.4921259842519685179 ) ) ;
#2372 = CARTESIAN_POINT ( 'NONE',  ( 0.3585568952266072751, -0.1763490727872195629, 0.3019338363380300039 ) ) ;
#2373 = ADVANCED_FACE ( 'NONE', ( #503 ), #1319, .T. ) ;
#2374 = ADVANCED_FACE ( 'NONE', ( #6760, #343 ), #2136, .T. ) ;
#2375 = DIRECTION ( 'NONE',  ( 0.3420201433256623291, 1.150791560227853228E-16, 0.9396926207859106484 ) ) ;
#2376 = FACE_OUTER_BOUND ( 'NONE', #3648, .T. ) ;
#2377 = CARTESIAN_POINT ( 'NONE',  ( -1.081428632361001396, -0.4470329974975803533, -1.553789141944099450 ) ) ;
#2378 = ADVANCED_FACE ( 'NONE', ( #3820 ), #2663, .T. ) ;
#2379 = DIRECTION ( 'NONE',  ( -1.000000000000000000, -0.000000000000000000, -4.625929269271482167E-15 ) ) ;
#2380 = VERTEX_POINT ( 'NONE', #5005 ) ;
#2381 = DIRECTION ( 'NONE',  ( 0.000000000000000000, 0.000000000000000000, -1.000000000000000000 ) ) ;
#2382 = VERTEX_POINT ( 'NONE', #2968 ) ;
#2383 = EDGE_CURVE ( 'NONE', #4290, #1140, #1281, .T. ) ;
#2384 = PRODUCT ( 'Supporter 2', 'Supporter 2', '', ( #2714 ) ) ;
#2385 = CARTESIAN_POINT ( 'NONE',  ( 0.3426144402833997127, -0.2904173629089126796, -0.1000635707556142007 ) ) ;
#2386 = DIRECTION ( 'NONE',  ( -7.708596820178695308E-30, 2.207829878515936732E-15, -1.000000000000000000 ) ) ;
#2387 = CARTESIAN_POINT ( 'NONE',  ( 0.3398315730591770500, -0.1188962366173021562, -0.2952755905511810774 ) ) ;
#2388 = EDGE_CURVE ( 'NONE', #6137, #3685, #6703, .T. ) ;
#2389 = AXIS2_PLACEMENT_3D ( 'NONE', #589, #2986, #1219 ) ;
#2390 = FACE_BOUND ( 'NONE', #3141, .T. ) ;
#2391 = CARTESIAN_POINT ( 'NONE',  ( -0.4514965799695756510, 0.9983959133492268379, -1.424958590981962203 ) ) ;
#2392 = CARTESIAN_POINT ( 'NONE',  ( 0.02637295201093723881, -0.1704774416898505729, -0.2952755905511810774 ) ) ;
#2393 = DIRECTION ( 'NONE',  ( 1.000000000000000000, 0.000000000000000000, 0.000000000000000000 ) ) ;
#2394 = LINE ( 'NONE', #2548, #835 ) ;
#2395 = CARTESIAN_POINT ( 'NONE',  ( -0.5073440712900673111, -0.9696655408444068147, -1.367310953805448426 ) ) ;
#2396 = CARTESIAN_POINT ( 'NONE',  ( 0.01178921041716320811, 0.1149842948508782436, 0.2952755905511810774 ) ) ;
#2397 = CARTESIAN_POINT ( 'NONE',  ( 0.000000000000000000, 0.2557161625347749712, -0.1476377952755909551 ) ) ;
#2398 = EDGE_LOOP ( 'NONE', ( #6597, #1227, #7274, #1653 ) ) ;
#2399 = DIRECTION ( 'NONE',  ( -0.000000000000000000, 0.000000000000000000, -1.000000000000000000 ) ) ;
#2400 = DIRECTION ( 'NONE',  ( 1.000000000000000000, 0.000000000000000000, 0.000000000000000000 ) ) ;
#2401 = VERTEX_POINT ( 'NONE', #5347 ) ;
#2402 = ORIENTED_EDGE ( 'NONE', *, *, #3413, .F. ) ;
#2403 = CARTESIAN_POINT ( 'NONE',  ( 0.3426022948973417859, 0.05819196463765207578, 0.3015401604570892014 ) ) ;
#2404=STYLED_ITEM('',(#7573),#4080);
#2405 = DIRECTION ( 'NONE',  ( -3.491481338843133750E-15, 1.000000000000000000, 0.000000000000000000 ) ) ;
#2406 = VERTEX_POINT ( 'NONE', #2514 ) ;
#2407 = CARTESIAN_POINT ( 'NONE',  ( 0.4720891361949481890, 0.9960021845704859489, -1.401719468380311362 ) ) ;
#2408 = AXIS2_PLACEMENT_3D ( 'NONE', #5885, #646, #2967 ) ;
#2409 = CARTESIAN_POINT ( 'NONE',  ( 2.892866454678787531E-17, 0.000000000000000000, 0.2362204724409449341 ) ) ;
#2410 = ORIENTED_EDGE ( 'NONE', *, *, #3982, .F. ) ;
#2411 = ORIENTED_EDGE ( 'NONE', *, *, #851, .F. ) ;
#2412 = LINE ( 'NONE', #1925, #5401 ) ;
#2413 = CARTESIAN_POINT ( 'NONE',  ( 0.3487098613656773316, 0.1177053732609037312, 0.3017042368166658051 ) ) ;
#2414 = APPLICATION_PROTOCOL_DEFINITION ( 'draft international standard', 'automotive_design', 1998, #4972 ) ;
#2415 = AXIS2_PLACEMENT_3D ( 'NONE', #6432, #4182, #4710 ) ;
#2416 = LENGTH_MEASURE_WITH_UNIT ( LENGTH_MEASURE( 0.02539999999999999897 ), #591 );
#2417 = CARTESIAN_POINT ( 'NONE',  ( 0.3543307086614173596, 0.03458999977076007010, -0.4082677165354332005 ) ) ;
#2418 = EDGE_LOOP ( 'NONE', ( #2099, #623 ) ) ;
#2419 = DIRECTION ( 'NONE',  ( 0.000000000000000000, 1.000000000000000000, 0.000000000000000000 ) ) ;
#2420 = CARTESIAN_POINT ( 'NONE',  ( 7.874015748031496287, 0.2559055118110236116, 0.4921259842519685179 ) ) ;
#2421 = EDGE_LOOP ( 'NONE', ( #4123, #6145, #6786 ) ) ;
#2422 = DIRECTION ( 'NONE',  ( 1.000000000000000000, 0.000000000000000000, -0.000000000000000000 ) ) ;
#2423 = EDGE_CURVE ( 'NONE', #4931, #3999, #2678, .T. ) ;
#2424 = ORIENTED_EDGE ( 'NONE', *, *, #3034, .T. ) ;
#2425 =( NAMED_UNIT ( * ) SI_UNIT ( $, .STERADIAN. ) SOLID_ANGLE_UNIT ( ) );
#2426 = CARTESIAN_POINT ( 'NONE',  ( 0.3496779274129793169, -0.1667266398149501727, -0.3017721699676331748 ) ) ;
#2427 = CARTESIAN_POINT ( 'NONE',  ( -1.085572738833922246, 0.4589124540220903548, -1.540322878613943125 ) ) ;
#2428 = CARTESIAN_POINT ( 'NONE',  ( 0.000000000000000000, 0.000000000000000000, -0.4072677165354330331 ) ) ;
#2429 = DIRECTION ( 'NONE',  ( 0.000000000000000000, 0.000000000000000000, 1.000000000000000000 ) ) ;
#2430 = ADVANCED_FACE ( 'NONE', ( #6539 ), #5852, .T. ) ;
#2431 = EDGE_CURVE ( 'NONE', #4413, #5853, #193, .T. ) ;
#2432 = CONICAL_SURFACE ( 'NONE', #1412, 0.2952755905511810774, 1.047197551196600518 ) ;
#2433 = UNCERTAINTY_MEASURE_WITH_UNIT (LENGTH_MEASURE( 1.000000000000000082E-05 ), #7500, 'distance_accuracy_value', 'NONE');
#2434 = CARTESIAN_POINT ( 'NONE',  ( 0.3574299024618896037, 0.1732824651941676231, 0.3001340337771135625 ) ) ;
#2435 = CARTESIAN_POINT ( 'NONE',  ( 0.4700904924197906176, -0.8785537298370117432, -1.433776001880362250 ) ) ;
#2436 = CARTESIAN_POINT ( 'NONE',  ( -1.044891351410288660, -0.4330708661417352334, -1.574550377471545470 ) ) ;
#2437 = CARTESIAN_POINT ( 'NONE',  ( 1.056523642887397862, 0.5141614760841569653, -1.484898342931014303 ) ) ;
#2438 = CARTESIAN_POINT ( 'NONE',  ( 0.02637295201093697167, 0.1704774416898497680, -0.2952755905511810774 ) ) ;
#2439 = DIRECTION ( 'NONE',  ( 0.000000000000000000, 0.5000000000000018874, 0.8660254037844375974 ) ) ;
#2440 = CARTESIAN_POINT ( 'NONE',  ( 0.000000000000000000, 0.000000000000000000, -0.4082677165354330340 ) ) ;
#2441 = LINE ( 'NONE', #1364, #3154 ) ;
#2442 = ORIENTED_EDGE ( 'NONE', *, *, #6090, .T. ) ;
#2443 = VECTOR ( 'NONE', #2375, 39.37007874015748143 ) ;
#2444 = CARTESIAN_POINT ( 'NONE',  ( -0.4713813068963899067, -1.084813395429188088, -1.526966363676886873 ) ) ;
#2445 = CARTESIAN_POINT ( 'NONE',  ( 1.048552902599916292, 0.4330708661417427274, -1.573978973432617279 ) ) ;
#2446 = CARTESIAN_POINT ( 'NONE',  ( 0.000000000000000000, 0.000000000000000000, 0.000000000000000000 ) ) ;
#2447 = DIRECTION ( 'NONE',  ( -0.000000000000000000, -0.000000000000000000, 1.000000000000000000 ) ) ;
#2448 = ORIENTED_EDGE ( 'NONE', *, *, #5803, .T. ) ;
#2449 = CARTESIAN_POINT ( 'NONE',  ( 0.5141614760841460852, 0.9609181420092316461, -1.361499588670819216 ) ) ;
#2450 = TOROIDAL_SURFACE ( 'NONE', #5871, 0.2948818897637794367, 0.05944881889763781874 ) ;
#2451 = ORIENTED_EDGE ( 'NONE', *, *, #5808, .T. ) ;
#2452 = PRODUCT ( 'hex flange bolt small_iso_ISO 4162 - M12 x 30 x 30-N', 'hex flange bolt small_iso_ISO 4162 - M12 x 30 x 30-N', '', ( #3063 ) ) ;
#2453 = CARTESIAN_POINT ( 'NONE',  ( 0.3496779274129793169, -0.1667266398149501727, -0.3017721699676331748 ) ) ;
#2454 = CARTESIAN_POINT ( 'NONE',  ( -0.1771653543307089573, 0.3068593950417301541, -0.4082677165354330340 ) ) ;
#2455 = ITEM_DEFINED_TRANSFORMATION ( 'NONE', 'NONE', #2937,  #5166 ) ;
#2456 = AXIS2_PLACEMENT_3D ( 'NONE', #1775, #3007, #1740 ) ;
#2457 = CARTESIAN_POINT ( 'NONE',  ( 0.02637295201093723881, -0.1704774416898505729, -0.2952755905511810774 ) ) ;
#2458 = FACE_OUTER_BOUND ( 'NONE', #5570, .T. ) ;
#2459 = ORIENTED_EDGE ( 'NONE', *, *, #7472, .T. ) ;
#2460 = DIRECTION ( 'NONE',  ( -0.000000000000000000, -1.000000000000000000, -0.000000000000000000 ) ) ;
#2461 = VERTEX_POINT ( 'NONE', #6048 ) ;
#2462 = DIRECTION ( 'NONE',  ( 3.491481338843133750E-15, -1.000000000000000000, -4.625929269271482167E-15 ) ) ;
#2463 = AXIS2_PLACEMENT_3D ( 'NONE', #7429, #6217, #6791 ) ;
#2464 = ORIENTED_EDGE ( 'NONE', *, *, #340, .T. ) ;
#2465 = B_SPLINE_CURVE_WITH_KNOTS ( 'NONE', 3,
 ( #2857, #2786, #1599, #2141 ),
 .UNSPECIFIED., .F., .F.,
 ( 4, 4 ),
 ( 0.000000000000000000, 0.0004815725036528544921 ),
 .UNSPECIFIED. ) ;
#2466 = DIRECTION ( 'NONE',  ( 0.000000000000000000, 0.000000000000000000, 1.000000000000000000 ) ) ;
#2467 = PRODUCT_RELATED_PRODUCT_CATEGORY ( 'part', '', ( #5872 ) ) ;
#2468 = CARTESIAN_POINT ( 'NONE',  ( 0.3543307086614173040, 0.1379824317933223410, -0.01414634932344265711 ) ) ;
#2469 = CARTESIAN_POINT ( 'NONE',  ( 0.4353079511162236126, 0.9479499796399308842, -1.456692913385826849 ) ) ;
#2470 = AXIS2_PLACEMENT_3D ( 'NONE', #2329, #1918, #7120 ) ;
#2471 = FACE_BOUND ( 'NONE', #5070, .T. ) ;
#2472 = CARTESIAN_POINT ( 'NONE',  ( 1.220472440944881720, 1.984939871850715226E-17, -0.9842519685039370358 ) ) ;
#2473 = VECTOR ( 'NONE', #474, 39.37007874015748143 ) ;
#2474 = APPLICATION_CONTEXT ( 'automotive_design' ) ;
#2475 = CARTESIAN_POINT ( 'NONE',  ( 0.4353079511162236126, -0.9479499796399308842, -1.456692913385826849 ) ) ;
#2476 = CARTESIAN_POINT ( 'NONE',  ( -0.4720891361949479115, 0.9960021845704875032, -1.401719468380313360 ) ) ;
#2477 = DIRECTION ( 'NONE',  ( 4.615976749461841764E-15, 0.000000000000000000, -1.000000000000000000 ) ) ;
#2478 = CARTESIAN_POINT ( 'NONE',  ( 0.000000000000000000, 0.000000000000000000, 0.4921259842519685179 ) ) ;
#2479 = EDGE_CURVE ( 'NONE', #5128, #4225, #4512, .T. ) ;
#2480 = EDGE_CURVE ( 'NONE', #2367, #4943, #2304, .T. ) ;
#2481 = DIRECTION ( 'NONE',  ( 0.000000000000000000, 0.000000000000000000, 1.000000000000000000 ) ) ;
#2482 = DIRECTION ( 'NONE',  ( 0.000000000000000000, -0.8660254037844381525, -0.5000000000000009992 ) ) ;
#2483 = CARTESIAN_POINT ( 'NONE',  ( 0.3485777078273625817, 0.2029921329169074307, 0.2518088348849962799 ) ) ;
#2484 = CARTESIAN_POINT ( 'NONE',  ( 0.3997746709170348356, 0.000000000000000000, 0.000000000000000000 ) ) ;
#2485 = DIRECTION ( 'NONE',  ( -0.000000000000000000, -1.000000000000000000, -0.000000000000000000 ) ) ;
#2486 = ORIENTED_EDGE ( 'NONE', *, *, #1439, .T. ) ;
#2487 = AXIS2_PLACEMENT_3D ( 'NONE', #954, #2102, #6910 ) ;
#2488 = CYLINDRICAL_SURFACE ( 'NONE', #5051, 0.2362204724409449619 ) ;
#2489 = DIRECTION ( 'NONE',  ( 0.000000000000000000, 0.000000000000000000, 1.000000000000000000 ) ) ;
#2490 = ORIENTED_EDGE ( 'NONE', *, *, #6507, .F. ) ;
#2491 = DIRECTION ( 'NONE',  ( 1.000000000000000000, 0.000000000000000000, 0.000000000000000000 ) ) ;
#2492 = EDGE_CURVE ( 'NONE', #3692, #1170, #952, .T. ) ;
#2493 = CARTESIAN_POINT ( 'NONE',  ( 0.000000000000000000, 2.957312202238506242E-17, 0.2952755905511810774 ) ) ;
#2494 = ORIENTED_EDGE ( 'NONE', *, *, #246, .F. ) ;
#2495 = DIRECTION ( 'NONE',  ( -0.000000000000000000, -0.000000000000000000, 1.000000000000000000 ) ) ;
#2496 = EDGE_LOOP ( 'NONE', ( #6165, #1970, #483, #397 ) ) ;
#2497 = ORIENTED_EDGE ( 'NONE', *, *, #6551, .F. ) ;
#2498 = CARTESIAN_POINT ( 'NONE',  ( 0.3398312250858251948, -0.3151631602416472555, -0.04467257488985885983 ) ) ;
#2499 = SURFACE_SIDE_STYLE ('',( #740 ) ) ;
#2500 = DIRECTION ( 'NONE',  ( -1.000000000000000000, -0.000000000000000000, -0.000000000000000000 ) ) ;
#2501 = ORIENTED_EDGE ( 'NONE', *, *, #4496, .T. ) ;
#2502 = ORIENTED_EDGE ( 'NONE', *, *, #4581, .F. ) ;
#2503 = DIRECTION ( 'NONE',  ( -1.000000000000000000, -0.000000000000000000, -0.000000000000000000 ) ) ;
#2504 = CARTESIAN_POINT ( 'NONE',  ( -0.4338950423154138147, -1.037563309807725043, -1.574803149606299302 ) ) ;
#2505 = ORIENTED_EDGE ( 'NONE', *, *, #329, .F. ) ;
#2506 = CARTESIAN_POINT ( 'NONE',  ( 0.3409812221349221573, -0.2754857644942658168, -0.1258275564122679768 ) ) ;
#2507 = CARTESIAN_POINT ( 'NONE',  ( -1.070856827570680903, 0.4375700189966262865, -1.565644132322242532 ) ) ;
#2508 = CARTESIAN_POINT ( 'NONE',  ( 0.000000000000000000, 0.000000000000000000, 0.000000000000000000 ) ) ;
#2509 = DIRECTION ( 'NONE',  ( -4.625929269271482167E-15, 0.000000000000000000, 1.000000000000000000 ) ) ;
#2510 = CARTESIAN_POINT ( 'NONE',  ( -1.651526287078852914E-15, 0.000000000000000000, -1.456692913385827515 ) ) ;
#2511 = CARTESIAN_POINT ( 'NONE',  ( 1.085749034841576810, 0.4630671888207514852, -1.535808138920396138 ) ) ;
#2512 = CARTESIAN_POINT ( 'NONE',  ( 0.3581828924050323715, 0.1743168766271107895, -0.3019256869348722061 ) ) ;
#2513 = DIRECTION ( 'NONE',  ( 0.000000000000000000, 0.000000000000000000, 1.000000000000000000 ) ) ;
#2514 = CARTESIAN_POINT ( 'NONE',  ( -0.2948818897637794922, 3.975280653137765506E-17, 0.1783464566929134354 ) ) ;
#2515 = FACE_OUTER_BOUND ( 'NONE', #7214, .T. ) ;
#2516 = EDGE_LOOP ( 'NONE', ( #6555, #4916, #3101, #5284 ) ) ;
#2517 = PRODUCT_DEFINITION_SHAPE ( 'NONE', 'NONE',  #7543 ) ;
#2518 = CARTESIAN_POINT ( 'NONE',  ( -0.9696655408442725887, 0.5073440712894341509, -1.367310953804909079 ) ) ;
#2519 = CARTESIAN_POINT ( 'NONE',  ( -0.4353079511162236681, 0.9479499796399324385, -1.456692913385828625 ) ) ;
#2520 = AXIS2_PLACEMENT_3D ( 'NONE', #5220, #6364, #5797 ) ;
#2521 = EDGE_CURVE ( 'NONE', #1603, #4753, #230, .T. ) ;
#2522 = EDGE_CURVE ( 'NONE', #1074, #5946, #4732, .T. ) ;
#2523 = ORIENTED_EDGE ( 'NONE', *, *, #946, .T. ) ;
#2524 = CARTESIAN_POINT ( 'NONE',  ( 0.3487105584742864473, -0.1177098269287414900, -0.3017042544367490309 ) ) ;
#2525 = EDGE_CURVE ( 'NONE', #1531, #2899, #1083, .T. ) ;
#2526 = FACE_OUTER_BOUND ( 'NONE', #2496, .T. ) ;
#2527 = ORIENTED_EDGE ( 'NONE', *, *, #2712, .T. ) ;
#2528 = CARTESIAN_POINT ( 'NONE',  ( 0.3411151615605715337, 0.2917056203871458142, -0.09774174715358552312 ) ) ;
#2529 = FACE_OUTER_BOUND ( 'NONE', #3183, .T. ) ;
#2530 = EDGE_CURVE ( 'NONE', #7296, #3756, #1569, .T. ) ;
#2531 = ADVANCED_FACE ( 'NONE', ( #112 ), #1192, .T. ) ;
#2532 = ORIENTED_EDGE ( 'NONE', *, *, #1029, .F. ) ;
#2533 = CARTESIAN_POINT ( 'NONE',  ( 0.3479980290963871625, -0.2016732288369692816, -0.2541005850305417257 ) ) ;
#2534 = ITEM_DEFINED_TRANSFORMATION ( 'NONE', 'NONE', #6981,  #5166 ) ;
#2535 = DIRECTION ( 'NONE',  ( -0.000000000000000000, -0.000000000000000000, 1.000000000000000000 ) ) ;
#2536 = AXIS2_PLACEMENT_3D ( 'NONE', #657, #618, #5357 ) ;
#2537 = CARTESIAN_POINT ( 'NONE',  ( -1.950024051643512521E-29, 1.861696953619914682E-15, -1.361499588670820771 ) ) ;
#2538 = B_SPLINE_CURVE_WITH_KNOTS ( 'NONE', 3,
 ( #2493, #6060, #808, #3176, #771, #3138 ),
 .UNSPECIFIED., .F., .F.,
 ( 4, 2, 4 ),
 ( 0.01227927579290655560, 0.01447189347357576844, 0.01666451115424498128 ),
 .UNSPECIFIED. ) ;
#2539 = EDGE_LOOP ( 'NONE', ( #217, #4517, #2361, #7258 ) ) ;
#2540 = VECTOR ( 'NONE', #5813, 39.37007874015748143 ) ;
#2541 = LINE ( 'NONE', #6182, #373 ) ;
#2542 = CARTESIAN_POINT ( 'NONE',  ( -1.063161251382700234, 0.4348450093584623755, -1.569784523562343770 ) ) ;
#2543 = CIRCLE ( 'NONE', #5975, 0.2362204724409448231 ) ;
#2544 = CARTESIAN_POINT ( 'NONE',  ( 0.4403524516313990222, -1.075169953371342801, -1.561970681382796045 ) ) ;
#2545 = CARTESIAN_POINT ( 'NONE',  ( 0.000000000000000000, 0.000000000000000000, -0.2952755905511810774 ) ) ;
#2546 = DIRECTION ( 'NONE',  ( -1.000000000000000000, -0.000000000000000000, 0.000000000000000000 ) ) ;
#2547 = AXIS2_PLACEMENT_3D ( 'NONE', #1869, #3626, #4817 ) ;
#2548 = CARTESIAN_POINT ( 'NONE',  ( -1.279527559055118280, 1.968503937007874072, 2.480314960629921295 ) ) ;
#2549 = DIRECTION ( 'NONE',  ( -1.000000000000000000, 0.000000000000000000, 0.000000000000000000 ) ) ;
#2550 = CARTESIAN_POINT ( 'NONE',  ( 0.3581828924050323715, 0.1743168766271109560, 0.3019256869348722616 ) ) ;
#2551 = CARTESIAN_POINT ( 'NONE',  ( 0.9842519685039370358, 0.7480314960629921295, 0.000000000000000000 ) ) ;
#2552 = DIRECTION ( 'NONE',  ( -1.000000000000000000, -1.045898529308444144E-14, 0.000000000000000000 ) ) ;
#2553 = ORIENTED_EDGE ( 'NONE', *, *, #2664, .F. ) ;
#2554 = CARTESIAN_POINT ( 'NONE',  ( 0.3432736861146661878, -0.3267484299055466446, 0.02460629921259842312 ) ) ;
#2555 = CARTESIAN_POINT ( 'NONE',  ( 0.2073490933073313947, -0.2894328052184282352, -0.4082677165354329785 ) ) ;
#2556 = AXIS2_PLACEMENT_3D ( 'NONE', #2954, #2878, #5295 ) ;
#2557 = CARTESIAN_POINT ( 'NONE',  ( -1.037563309807723488, -0.4338950423154175340, -1.574803149606299302 ) ) ;
#2558 = CARTESIAN_POINT ( 'NONE',  ( -0.4333661275892074505, -1.041228047528454770, -1.574803149606299302 ) ) ;
#2559 = CARTESIAN_POINT ( 'NONE',  ( 0.3485616995351332181, 0.1165012447190262312, 0.3017003685801735724 ) ) ;
#2560 = AXIS2_PLACEMENT_3D ( 'NONE', #5619, #2696, #2621 ) ;
#2561 = ADVANCED_FACE ( 'NONE', ( #4774 ), #3524, .T. ) ;
#2562 = DIRECTION ( 'NONE',  ( -1.000000000000000000, -0.000000000000000000, -0.000000000000000000 ) ) ;
#2563 = EDGE_LOOP ( 'NONE', ( #1887, #4363, #863, #619, #586, #5239 ) ) ;
#2564 = CARTESIAN_POINT ( 'NONE',  ( 0.3505602286436571013, -0.1704774416898497957, 0.2952755905511814660 ) ) ;
#2565 = ORIENTED_EDGE ( 'NONE', *, *, #3880, .F. ) ;
#2566 = ORIENTED_EDGE ( 'NONE', *, *, #1542, .F. ) ;
#2567 = DIRECTION ( 'NONE',  ( -0.000000000000000000, -1.000000000000000000, -0.000000000000000000 ) ) ;
#2568 = EDGE_CURVE ( 'NONE', #5974, #5935, #5244, .T. ) ;
#2569 = EDGE_CURVE ( 'NONE', #3513, #6033, #1694, .T. ) ;
#2570 = B_SPLINE_CURVE_WITH_KNOTS ( 'NONE', 3,
 ( #1303, #2417, #5292, #2948, #1758, #131 ),
 .UNSPECIFIED., .F., .F.,
 ( 4, 2, 4 ),
 ( 0.01452727543195640389, 0.01715716534226973539, 0.01978705525258306688 ),
 .UNSPECIFIED. ) ;
#2571 = CARTESIAN_POINT ( 'NONE',  ( 0.3391216574609289269, 0.1954800165277119361, 0.2519698606119610829 ) ) ;
#2572 = ORIENTED_EDGE ( 'NONE', *, *, #1731, .T. ) ;
#2573 = CIRCLE ( 'NONE', #4411, 0.3543307086614173596 ) ;
#2574 = CARTESIAN_POINT ( 'NONE',  ( -0.3543307086614173040, -0.2045729300278205931, -0.3766201741223081378 ) ) ;
#2575 = ORIENTED_EDGE ( 'NONE', *, *, #6353, .T. ) ;
#2576 = ADVANCED_BREP_SHAPE_REPRESENTATION ( '', ( #4033, #5166 ), #7344 ) ;
#2577 = CARTESIAN_POINT ( 'NONE',  ( -0.2952755905511811885, 0.000000000000000000, -0.7983802283864783744 ) ) ;
#2578 = EDGE_CURVE ( 'NONE', #811, #443, #2142, .T. ) ;
#2579 = ORIENTED_EDGE ( 'NONE', *, *, #5791, .T. ) ;
#2580 = AXIS2_PLACEMENT_3D ( 'NONE', #4280, #7331, #4937 ) ;
#2581 = PRODUCT_DEFINITION_SHAPE ( 'NONE', 'NONE',  #2700 ) ;
#2582 = CARTESIAN_POINT ( 'NONE',  ( 0.01171324505787542034, 0.1984117137466533121, -0.2468920120763460069 ) ) ;
#2583 = CARTESIAN_POINT ( 'NONE',  ( 1.015122112586412939, -0.2347042945180431994, -0.9558637132201285302 ) ) ;
#2584 = CARTESIAN_POINT ( 'NONE',  ( -0.9346848099469026172, -0.4388997119412576531, -1.455943619906243436 ) ) ;
#2585 = AXIS2_PLACEMENT_3D ( 'NONE', #6099, #2643, #2150 ) ;
#2586 = CYLINDRICAL_SURFACE ( 'NONE', #4647, 0.2362204724409448231 ) ;
#2587 = AXIS2_PLACEMENT_3D ( 'NONE', #5875, #27, #4685 ) ;
#2588 = FACE_OUTER_BOUND ( 'NONE', #4055, .T. ) ;
#2589 = CARTESIAN_POINT ( 'NONE',  ( 0.0006233585804808155053, 0.2702164766613434077, 0.1225225144826656842 ) ) ;
#2590 = CARTESIAN_POINT ( 'NONE',  ( 7.874015748031496287, 0.2559055118110236116, 0.000000000000000000 ) ) ;
#2591 = CARTESIAN_POINT ( 'NONE',  ( 1.030265555772306829, 0.4349482935633184333, -1.574803149606299302 ) ) ;
#2592 = CARTESIAN_POINT ( 'NONE',  ( -0.8785537298370117432, -0.4700904924197938373, -1.433776001880364470 ) ) ;
#2593 = ORIENTED_EDGE ( 'NONE', *, *, #6368, .T. ) ;
#2594 = CARTESIAN_POINT ( 'NONE',  ( 0.3483227611829846637, -0.1704774416898499345, 0.2952755905511811330 ) ) ;
#2595 = CARTESIAN_POINT ( 'NONE',  ( -0.4756000659977974721, 1.083679028610380346, -1.522578585053779410 ) ) ;
#2596 = ORIENTED_EDGE ( 'NONE', *, *, #5431, .T. ) ;
#2597 = CARTESIAN_POINT ( 'NONE',  ( 0.3505601438611538057, 0.1704774416898496292, -0.2952755905511812995 ) ) ;
#2598 = CARTESIAN_POINT ( 'NONE',  ( -0.4338950423154138147, -1.037563309807725043, -1.574803149606299302 ) ) ;
#2599 = VECTOR ( 'NONE', #6532, 39.37007874015748143 ) ;
#2600 = CARTESIAN_POINT ( 'NONE',  ( 0.000000000000000000, -0.2557161625347750822, -0.1476377952755907330 ) ) ;
#2601 = ORIENTED_EDGE ( 'NONE', *, *, #4154, .T. ) ;
#2602 = VECTOR ( 'NONE', #2135, 39.37007874015748143 ) ;
#2603 = CARTESIAN_POINT ( 'NONE',  ( 0.4349482548737268472, -1.030265823844198625, -1.574803149606299524 ) ) ;
#2604 = EDGE_LOOP ( 'NONE', ( #4956, #4865 ) ) ;
#2605 = EDGE_CURVE ( 'NONE', #4697, #96, #5979, .T. ) ;
#2606 = CARTESIAN_POINT ( 'NONE',  ( 0.3997746709170348356, 5.668966274263039413E-17, 0.4629062255509093782 ) ) ;
#2607 = CARTESIAN_POINT ( 'NONE',  ( 0.3527006543068526567, -0.3418446578861590868, 8.418741006566202135E-18 ) ) ;
#2608 = CARTESIAN_POINT ( 'NONE',  ( -0.05817553349160980991, -0.3755582001340100895, -0.01402797064541895684 ) ) ;
#2609 = ORIENTED_EDGE ( 'NONE', *, *, #3704, .F. ) ;
#2610 = CARTESIAN_POINT ( 'NONE',  ( 1.083410700381150393, -0.4508657589754589967, -1.549345605342071774 ) ) ;
#2611 = DIRECTION ( 'NONE',  ( 1.000000000000000000, 0.000000000000000000, 0.000000000000000000 ) ) ;
#2612 = ORIENTED_EDGE ( 'NONE', *, *, #7191, .F. ) ;
#2613 = CLOSED_SHELL ( 'NONE', ( #441, #200, #5016, #7105, #9, #807, #2378, #3180, #4762, #2624, #2561, #5521, #201, #6275, #1585, #2838, #6000, #3930, #4529, #5195, #6970, #6684, #6592, #156, #6880, #5060, #1716, #5330, #3464, #1723, #440, #5199, #2531, #525, #1969, #3840, #6402, #4875, #893, #6683, #377 ) ) ;
#2614 = DIRECTION ( 'NONE',  ( 0.000000000000000000, 0.000000000000000000, 1.000000000000000000 ) ) ;
#2615 = EDGE_CURVE ( 'NONE', #7028, #4474, #4135, .T. ) ;
#2616 = ORIENTED_EDGE ( 'NONE', *, *, #3081, .T. ) ;
#2617 = EDGE_CURVE ( 'NONE', #4891, #6130, #3653, .T. ) ;
#2618 =( NAMED_UNIT ( * ) PLANE_ANGLE_UNIT ( ) SI_UNIT ( $, .RADIAN. ) );
#2619 = AXIS2_PLACEMENT_3D ( 'NONE', #6397, #624, #7003 ) ;
#2620 = EDGE_CURVE ( 'NONE', #1688, #7237, #3162, .T. ) ;
#2621 = DIRECTION ( 'NONE',  ( 0.000000000000000000, 0.000000000000000000, 1.000000000000000000 ) ) ;
#2622 = DIRECTION ( 'NONE',  ( -1.000000000000000000, 0.000000000000000000, 0.000000000000000000 ) ) ;
#2623 = CARTESIAN_POINT ( 'NONE',  ( 0.7719899816204534027, 0.1048018568659492278, -0.9787612993317383880 ) ) ;
#2624 = ADVANCED_FACE ( 'NONE', ( #6082 ), #849, .T. ) ;
#2625 = CARTESIAN_POINT ( 'NONE',  ( 0.3306743754077733910, -1.707404996040164512E-17, 0.2952755905511811885 ) ) ;
#2626 = CARTESIAN_POINT ( 'NONE',  ( 0.3527006543068523237, 0.1709223289430787940, -0.2960461578774135072 ) ) ;
#2627 = CARTESIAN_POINT ( 'NONE',  ( 1.048552902599924730, -0.4330708661417213001, -1.573978973432616835 ) ) ;
#2628 = DIRECTION ( 'NONE',  ( 1.000000000000000000, 0.000000000000000000, 0.000000000000000000 ) ) ;
#2629 = ORIENTED_EDGE ( 'NONE', *, *, #6273, .T. ) ;
#2630 = CARTESIAN_POINT ( 'NONE',  ( -0.9726683636255533116, 0.4332839536939371294, -1.452651081959918766 ) ) ;
#2631 = CARTESIAN_POINT ( 'NONE',  ( 0.3561392902752972267, 0.3446605091515489439, -2.917830865379561131E-17 ) ) ;
#2632 = DIRECTION ( 'NONE',  ( 0.000000000000000000, 0.000000000000000000, 1.000000000000000000 ) ) ;
#2633 = B_SPLINE_CURVE_WITH_KNOTS ( 'NONE', 3,
 ( #892, #1963, #3221, #7345, #3763, #7233 ),
 .UNSPECIFIED., .F., .F.,
 ( 4, 2, 4 ),
 ( 2.380730968201100790E-07, 0.002629065763328349622, 0.005257893453559878486 ),
 .UNSPECIFIED. ) ;
#2634 = CARTESIAN_POINT ( 'NONE',  ( 0.3321025531238107620, -0.02909241602403181068, -0.2952755905511810774 ) ) ;
#2635 = CARTESIAN_POINT ( 'NONE',  ( 0.000000000000000000, 0.000000000000000000, 0.3732633159281743551 ) ) ;
#2636 = CARTESIAN_POINT ( 'NONE',  ( 0.000000000000000000, 0.000000000000000000, 0.000000000000000000 ) ) ;
#2637 = ORIENTED_EDGE ( 'NONE', *, *, #3416, .T. ) ;
#2638 = VECTOR ( 'NONE', #5288, 39.37007874015748143 ) ;
#2639 = CARTESIAN_POINT ( 'NONE',  ( 0.3581828924050323715, -0.1743168766271109560, 0.3019256869348722616 ) ) ;
#2640 = ORIENTED_EDGE ( 'NONE', *, *, #6603, .T. ) ;
#2641 = PRODUCT_DEFINITION_SHAPE ( 'NONE', 'NONE',  #558 ) ;
#2642 = ORIENTED_EDGE ( 'NONE', *, *, #3467, .T. ) ;
#2643 = DIRECTION ( 'NONE',  ( 0.000000000000000000, 1.000000000000000000, 0.000000000000000000 ) ) ;
#2644 = CARTESIAN_POINT ( 'NONE',  ( 0.3483227611829849413, -0.3409548833797009237, 0.000000000000000000 ) ) ;
#2645 = CARTESIAN_POINT ( 'NONE',  ( 0.9696319393320019797, -0.5073702590894858533, -1.367288630523686210 ) ) ;
#2646 = ORIENTED_EDGE ( 'NONE', *, *, #1033, .T. ) ;
#2647 = CARTESIAN_POINT ( 'NONE',  ( 0.7495315129468413939, 0.03083906941738260785, 0.9838885550255186407 ) ) ;
#2648 = ORIENTED_EDGE ( 'NONE', *, *, #5676, .F. ) ;
#2649 = ORIENTED_EDGE ( 'NONE', *, *, #3070, .F. ) ;
#2650 = CARTESIAN_POINT ( 'NONE',  ( 26.34267259271975092, 45.20863634146751764, 53.38200498105501168 ) ) ;
#2651 = CIRCLE ( 'NONE', #5107, 0.4921259842519685179 ) ;
#2652 = CARTESIAN_POINT ( 'NONE',  ( 3.027559055118110187, 0.000000000000000000, 0.000000000000000000 ) ) ;
#2653 = CARTESIAN_POINT ( 'NONE',  ( 0.2362204724409449619, 2.892866454678788147E-17, -0.4072677165354330331 ) ) ;
#2654 = LENGTH_MEASURE_WITH_UNIT ( LENGTH_MEASURE( 0.02539999999999999897 ), #865 );
#2655 = EDGE_CURVE ( 'NONE', #6508, #655, #2792, .T. ) ;
#2656 = CARTESIAN_POINT ( 'NONE',  ( 0.1771653543307089296, 0.3068593950417301541, -0.4082677165354330340 ) ) ;
#2657 = CARTESIAN_POINT ( 'NONE',  ( 0.8062392625377295952, 0.1560493051692869171, -0.9718662726019896558 ) ) ;
#2658 = AXIS2_PLACEMENT_3D ( 'NONE', #1201, #1777, #6413 ) ;
#2659 = DIRECTION ( 'NONE',  ( 0.000000000000000000, -1.000000000000000000, -2.095133389269358970E-15 ) ) ;
#2660 = CARTESIAN_POINT ( 'NONE',  ( 0.3483227611829846082, 0.1704774416898497680, -0.2952755905511810774 ) ) ;
#2661 = B_SPLINE_CURVE_WITH_KNOTS ( 'NONE', 3,
 ( #2472, #4808, #5427, #1860, #3160, #790, #1315, #5506, #1902, #2777, #2206, #417, #2740, #1461, #1544, #4468, #4537, #5081, #3351, #4386, #4427, #5625, #6871, #6756, #3387, #7398, #3970, #5703, #6298, #338, #1053, #5734, #1505, #2657, #3852, #6186, #2623, #375, #4960, #5044, #6332, #2845, #2345, #1764 ),
 .UNSPECIFIED., .F., .F.,
 ( 4, 2, 2, 2, 2, 2, 2, 2, 2, 2, 2, 2, 2, 2, 2, 2, 2, 2, 2, 2, 2, 4 ),
 ( 4.896973959386981381E-19, 0.001176728898091255592, 0.001765093347136882304, 0.002353457796182509016, 0.003530186694273764608, 0.004706915592365020634, 0.005883644490456278395, 0.007060373388547535288, 0.007648737837593169372, 0.008237102286638802590, 0.009413831184730070759, 0.01059056008282133893, 0.01176728898091260710, 0.01235565342995824031, 0.01294401787900387527, 0.01353238232804950848, 0.01412074677709514170, 0.01529747567518641160, 0.01647420457327768151, 0.01765093347136895141, 0.01823929792041458289, 0.01882766236946021784 ),
 .UNSPECIFIED. ) ;
#2662 = CIRCLE ( 'NONE', #6216, 0.1982677165354330695 ) ;
#2663 = CYLINDRICAL_SURFACE ( 'NONE', #4743, 0.2362204724409449341 ) ;
#2664 = EDGE_CURVE ( 'NONE', #2899, #2106, #505, .T. ) ;
#2665 = FACE_OUTER_BOUND ( 'NONE', #2685, .T. ) ;
#2666 = EDGE_CURVE ( 'NONE', #2214, #283, #5528, .T. ) ;
#2667 = ORIENTED_EDGE ( 'NONE', *, *, #481, .T. ) ;
#2668 = FACE_OUTER_BOUND ( 'NONE', #5310, .T. ) ;
#2669 = ORIENTED_EDGE ( 'NONE', *, *, #256, .F. ) ;
#2670 = CARTESIAN_POINT ( 'NONE',  ( 1.649606299212598381, 0.000000000000000000, 0.000000000000000000 ) ) ;
#2671 = CARTESIAN_POINT ( 'NONE',  ( 0.3337358785015786533, -0.05918271685993679171, -0.2952755905511810774 ) ) ;
#2672 = CONTEXT_DEPENDENT_SHAPE_REPRESENTATION ( #3157, #3684 ) ;
#2673 = CARTESIAN_POINT ( 'NONE',  ( -0.9783380834473003329, -0.4342018836190635334, -1.450123305573145505 ) ) ;
#2674 = EDGE_LOOP ( 'NONE', ( #887, #7384, #2616, #5981, #4968 ) ) ;
#2675 = AXIS2_PLACEMENT_3D ( 'NONE', #6466, #1837, #2982 ) ;
#2676 = LINE ( 'NONE', #6062, #7473 ) ;
#2677 = ORIENTED_EDGE ( 'NONE', *, *, #145, .F. ) ;
#2678 = B_SPLINE_CURVE_WITH_KNOTS ( 'NONE', 3,
 ( #3669, #4275, #724, #5930, #3090, #5393 ),
 .UNSPECIFIED., .F., .F.,
 ( 4, 2, 4 ),
 ( 0.009270618776430220032, 0.01189894710419331196, 0.01452727543195640389 ),
 .UNSPECIFIED. ) ;
#2679 = ORIENTED_EDGE ( 'NONE', *, *, #49, .F. ) ;
#2680 = DIRECTION ( 'NONE',  ( 1.000000000000000000, 0.000000000000000000, 0.000000000000000000 ) ) ;
#2681 = CIRCLE ( 'NONE', #3175, 0.2362204724409449341 ) ;
#2682 = CARTESIAN_POINT ( 'NONE',  ( -1.044891351410289548, 0.4330708661417286276, -1.574550377471545692 ) ) ;
#2683 = ORIENTED_EDGE ( 'NONE', *, *, #4541, .T. ) ;
#2684 = CARTESIAN_POINT ( 'NONE',  ( 0.3496779274129791504, 0.1667266398149495066, 0.3017721699676332303 ) ) ;
#2685 = EDGE_LOOP ( 'NONE', ( #6897, #6812, #4628, #1207 ) ) ;
#2686 = DIRECTION ( 'NONE',  ( -3.491481338843133750E-15, 1.000000000000000000, 0.000000000000000000 ) ) ;
#2687 = EDGE_LOOP ( 'NONE', ( #4252, #5217, #170, #5144, #5057 ) ) ;
#2688 = MECHANICAL_DESIGN_GEOMETRIC_PRESENTATION_REPRESENTATION (  '', ( #5996 ), #3429 ) ;
#2689 =( NAMED_UNIT ( * ) SI_UNIT ( $, .STERADIAN. ) SOLID_ANGLE_UNIT ( ) );
#2690 = ORIENTED_EDGE ( 'NONE', *, *, #246, .T. ) ;
#2691 = ORIENTED_EDGE ( 'NONE', *, *, #1876, .T. ) ;
#2692 = CARTESIAN_POINT ( 'NONE',  ( -0.4921259842519648542, 0.000000000000000000, -2.204724409448822975 ) ) ;
#2693 = CARTESIAN_POINT ( 'NONE',  ( 33.89456220083551585, 40.86510553865259254, 54.13003647711801136 ) ) ;
#2694 = AXIS2_PLACEMENT_3D ( 'NONE', #784, #5373, #3610 ) ;
#2695 = FACE_OUTER_BOUND ( 'NONE', #2760, .T. ) ;
#2696 = DIRECTION ( 'NONE',  ( 0.000000000000000000, 1.000000000000000000, 0.000000000000000000 ) ) ;
#2697 = CARTESIAN_POINT ( 'NONE',  ( 0.8280287984149673486, -0.1778526427332735582, -0.9681128863842415333 ) ) ;
#2698 = CARTESIAN_POINT ( 'NONE',  ( -0.3543307086614173040, 0.1714946277491101179, -0.3861690574847828072 ) ) ;
#2699 = CIRCLE ( 'NONE', #5999, 1.089828288828796676 ) ;
#2700 = PRODUCT_DEFINITION ( 'UNKNOWN', '', #3495, #4194 ) ;
#2701 = LENGTH_MEASURE_WITH_UNIT ( LENGTH_MEASURE( 0.02539999999999999897 ), #3932 );
#2702 = CARTESIAN_POINT ( 'NONE',  ( 0.02637295201093751290, -0.3409548833797009237, -9.138209691400258722E-18 ) ) ;
#2703 = AXIS2_PLACEMENT_3D ( 'NONE', #1237, #3586, #2477 ) ;
#2704 = CARTESIAN_POINT ( 'NONE',  ( 0.3565325103478088065, -0.3440765519545064266, -0.005406888575953978406 ) ) ;
#2705 = CARTESIAN_POINT ( 'NONE',  ( -3.198568410424924124, 2.407012729153881203, 2.480314960629921295 ) ) ;
#2706 = AXIS2_PLACEMENT_3D ( 'NONE', #7201, #4996, #4420 ) ;
#2707 = FACE_OUTER_BOUND ( 'NONE', #1417, .T. ) ;
#2708 = AXIS2_PLACEMENT_3D ( 'NONE', #1145, #6437, #4608 ) ;
#2709 = ORIENTED_EDGE ( 'NONE', *, *, #4538, .T. ) ;
#2710 = CARTESIAN_POINT ( 'NONE',  ( -0.9842519685039370358, 1.220472440944881942, 0.4724409448818898127 ) ) ;
#2711 = EDGE_CURVE ( 'NONE', #4601, #5274, #1803, .T. ) ;
#2712 = EDGE_CURVE ( 'NONE', #2380, #1045, #91, .T. ) ;
#2713 = CARTESIAN_POINT ( 'NONE',  ( 0.1922007978147437512, 0.2981786776988370469, -0.4082677165354333670 ) ) ;
#2714 = PRODUCT_CONTEXT ( 'NONE', #286, 'mechanical' ) ;
#2715 = EDGE_CURVE ( 'NONE', #18, #448, #1847, .T. ) ;
#2716 = CARTESIAN_POINT ( 'NONE',  ( -0.9810555383103370941, -0.4349192646538896367, -1.448591292758283799 ) ) ;
#2717 = EDGE_LOOP ( 'NONE', ( #5204, #7489, #44, #6736, #1007, #291 ) ) ;
#2718 = VECTOR ( 'NONE', #2917, 39.37007874015748143 ) ;
#2719 = CARTESIAN_POINT ( 'NONE',  ( 1.051607560569809863, -0.4330708661417213001, -1.573502278225820561 ) ) ;
#2720 = CARTESIAN_POINT ( 'NONE',  ( 0.3510872220068100846, -0.1819230426404178091, 0.2754512281816298147 ) ) ;
#2721 = ORIENTED_EDGE ( 'NONE', *, *, #3984, .T. ) ;
#2722 = EDGE_LOOP ( 'NONE', ( #1495, #206, #839, #6680 ) ) ;
#2723 = ADVANCED_FACE ( 'NONE', ( #1663 ), #4667, .F. ) ;
#2724 = VECTOR ( 'NONE', #2901, 39.37007874015748143 ) ;
#2725 = CARTESIAN_POINT ( 'NONE',  ( 0.000000000000000000, 1.496062992125984259, -0.2362204724409449341 ) ) ;
#2726 = CARTESIAN_POINT ( 'NONE',  ( -0.4330708661417322913, 0.9604263920613194117, -1.456063616177416087 ) ) ;
#2727 = DIRECTION ( 'NONE',  ( -0.000000000000000000, -0.000000000000000000, 1.000000000000000000 ) ) ;
#2728 = ORIENTED_EDGE ( 'NONE', *, *, #3748, .T. ) ;
#2729 = CARTESIAN_POINT ( 'NONE',  ( 0.3581828924050323715, 0.1743168766271109560, 0.3019256869348722616 ) ) ;
#2730 = ORIENTED_EDGE ( 'NONE', *, *, #2664, .T. ) ;
#2731 = CARTESIAN_POINT ( 'NONE',  ( -0.3254211578371892788, -0.2212638669783397183, -0.3862566910637255102 ) ) ;
#2732 = VERTEX_POINT ( 'NONE', #4093 ) ;
#2733 = ORIENTED_EDGE ( 'NONE', *, *, #5801, .F. ) ;
#2734 = ORIENTED_EDGE ( 'NONE', *, *, #1670, .T. ) ;
#2735 = DIRECTION ( 'NONE',  ( -3.899598398114372558E-16, 7.046558751726398440E-19, 1.000000000000000000 ) ) ;
#2736 = LINE ( 'NONE', #3266, #5011 ) ;
#2737 = CARTESIAN_POINT ( 'NONE',  ( 0.4685039370078740717, 2.892866454678787531E-17, -0.2362204724409449064 ) ) ;
#2738 = AXIS2_PLACEMENT_3D ( 'NONE', #7059, #6409, #4649 ) ;
#2739 = DIRECTION ( 'NONE',  ( 0.000000000000000000, 1.000000000000000000, 0.000000000000000000 ) ) ;
#2740 = CARTESIAN_POINT ( 'NONE',  ( 1.128523761465410891, 0.1876879802734073011, -0.9662312300142489319 ) ) ;
#2741 = DIRECTION ( 'NONE',  ( 1.000000000000000000, 0.000000000000000000, 0.000000000000000000 ) ) ;
#2742 = CARTESIAN_POINT ( 'NONE',  ( 0.3574269917172681610, 0.1732784665916975442, -0.3001271079942677833 ) ) ;
#2743 = DIRECTION ( 'NONE',  ( -0.000000000000000000, -0.000000000000000000, 1.000000000000000000 ) ) ;
#2744 = CARTESIAN_POINT ( 'NONE',  ( 1.968503937007874072, 1.496062992125984259, 0.000000000000000000 ) ) ;
#2745 = PRODUCT_DEFINITION ( 'UNKNOWN', '', #3750, #63 ) ;
#2746 = EDGE_LOOP ( 'NONE', ( #7456, #6115, #6277, #511 ) ) ;
#2747 = DIRECTION ( 'NONE',  ( -1.000000000000000000, 0.000000000000000000, 0.000000000000000000 ) ) ;
#2748 = DIRECTION ( 'NONE',  ( 0.000000000000000000, 0.000000000000000000, 1.000000000000000000 ) ) ;
#2749 = DIRECTION ( 'NONE',  ( -0.5000000000000006661, -0.8660254037844383745, 0.000000000000000000 ) ) ;
#2750 = B_SPLINE_CURVE_WITH_KNOTS ( 'NONE', 3,
 ( #2344, #6976, #2274, #55, #1182, #593, #5294, #3463, #5832 ),
 .UNSPECIFIED., .F., .F.,
 ( 4, 2, 1, 2, 4 ),
 ( 2.312923578716022130E-20, 0.002165063509461098365, 0.004330127018922196730, 0.006495190528383295095, 0.008660254037844393460 ),
 .UNSPECIFIED. ) ;
#2751 = ORIENTED_EDGE ( 'NONE', *, *, #4435, .F. ) ;
#2752 = CARTESIAN_POINT ( 'NONE',  ( 0.3337354549120237213, 0.2261274626982069103, -0.1988869267224314119 ) ) ;
#2753 = DIRECTION ( 'NONE',  ( 0.000000000000000000, 0.000000000000000000, 1.000000000000000000 ) ) ;
#2754 = EDGE_CURVE ( 'NONE', #3441, #1383, #1696, .T. ) ;
#2755 = ORIENTED_EDGE ( 'NONE', *, *, #5938, .F. ) ;
#2756 = ORIENTED_EDGE ( 'NONE', *, *, #2294, .F. ) ;
#2757 = FACE_OUTER_BOUND ( 'NONE', #1325, .T. ) ;
#2758 = DIRECTION ( 'NONE',  ( 0.000000000000000000, 0.000000000000000000, -1.000000000000000000 ) ) ;
#2759 = CARTESIAN_POINT ( 'NONE',  ( -0.2699662542182227343, 3.306133091061471023E-17, 0.1783464566929134354 ) ) ;
#2760 = EDGE_LOOP ( 'NONE', ( #554, #2464, #7485 ) ) ;
#2761 = CARTESIAN_POINT ( 'NONE',  ( -0.7480314960629922405, 1.220472440944881942, 0.4724409448818898127 ) ) ;
#2762 = VERTEX_POINT ( 'NONE', #5825 ) ;
#2763 = DIRECTION ( 'NONE',  ( -0.000000000000000000, -0.000000000000000000, 1.000000000000000000 ) ) ;
#2764 = EDGE_CURVE ( 'NONE', #4703, #7025, #499, .T. ) ;
#2765 = ADVANCED_FACE ( 'NONE', ( #6425 ), #4131, .F. ) ;
#2766 = CARTESIAN_POINT ( 'NONE',  ( 0.3565422270302657237, 0.3441025489056184772, -0.005451916616122978385 ) ) ;
#2767 = VERTEX_POINT ( 'NONE', #2409 ) ;
#2768 = DIMENSIONAL_EXPONENTS ( 1.000000000000000000, 0.000000000000000000, 0.000000000000000000, 0.000000000000000000, 0.000000000000000000, 0.000000000000000000, 0.000000000000000000 ) ;
#2769 = EDGE_CURVE ( 'NONE', #4410, #1296, #1188, .T. ) ;
#2770 =( REPRESENTATION_RELATIONSHIP ('NONE','NONE', #303, #5265 ) REPRESENTATION_RELATIONSHIP_WITH_TRANSFORMATION ( #4198 )SHAPE_REPRESENTATION_RELATIONSHIP( ) );
#2771 = ORIENTED_EDGE ( 'NONE', *, *, #376, .F. ) ;
#2772 = CARTESIAN_POINT ( 'NONE',  ( 2.834645669291338432, 0.000000000000000000, 0.4724409448818898127 ) ) ;
#2773 = CARTESIAN_POINT ( 'NONE',  ( 18.30767084474955197, 38.73487850452738002, 54.13003647711800426 ) ) ;
#2774 = DIRECTION ( 'NONE',  ( -2.207829878515936732E-15, 0.000000000000000000, 1.000000000000000000 ) ) ;
#2775 = LINE ( 'NONE', #5157, #4012 ) ;
#2776 = CARTESIAN_POINT ( 'NONE',  ( -0.3543307086614173596, 0.03458999977076020194, -0.4082677165354332005 ) ) ;
#2777 = CARTESIAN_POINT ( 'NONE',  ( 1.172031980416358365, 0.1441408498666779114, -0.9737261629585141076 ) ) ;
#2778 = AXIS2_PLACEMENT_3D ( 'NONE', #6322, #6782, #1004 ) ;
#2779 = DIRECTION ( 'NONE',  ( 0.000000000000000000, 0.000000000000000000, 1.000000000000000000 ) ) ;
#2780 = CARTESIAN_POINT ( 'NONE',  ( 0.3465694189147059956, -0.1966695024996656382, 0.2499096104736426016 ) ) ;
#2781 = CARTESIAN_POINT ( 'NONE',  ( 0.000000000000000000, 0.000000000000000000, -0.4082677165354330340 ) ) ;
#2782 = AXIS2_PLACEMENT_3D ( 'NONE', #2636, #1955, #6122 ) ;
#2783 = DIRECTION ( 'NONE',  ( 1.000000000000000000, 0.000000000000000000, 2.207829878515936732E-15 ) ) ;
#2784 = ORIENTED_EDGE ( 'NONE', *, *, #1146, .T. ) ;
#2785 = CARTESIAN_POINT ( 'NONE',  ( 0.4342018836190599251, -0.9783380834472997778, -1.450123305573142840 ) ) ;
#2786 = CARTESIAN_POINT ( 'NONE',  ( 0.9541934910893076216, -0.4339190921229351683, -1.456692913385826849 ) ) ;
#2787 = CIRCLE ( 'NONE', #3771, 0.4921259842519685179 ) ;
#2788 = CONTEXT_DEPENDENT_SHAPE_REPRESENTATION ( #6824, #1839 ) ;
#2789 = DIRECTION ( 'NONE',  ( -4.625929269271482167E-15, 0.000000000000000000, 1.000000000000000000 ) ) ;
#2790 = ORIENTED_EDGE ( 'NONE', *, *, #5803, .F. ) ;
#2791 = CARTESIAN_POINT ( 'NONE',  ( 0.3585665126877354281, -0.1732820025503174766, 0.3037348580927970443 ) ) ;
#2792 = CIRCLE ( 'NONE', #844, 0.2362204724409448231 ) ;
#2793 = ORIENTED_EDGE ( 'NONE', *, *, #4590, .F. ) ;
#2794 = ORIENTED_EDGE ( 'NONE', *, *, #5242, .T. ) ;
#2795 = CARTESIAN_POINT ( 'NONE',  ( 0.3543307086614173040, 0.2045729300278205931, -0.03164754241312491001 ) ) ;
#2796 = CARTESIAN_POINT ( 'NONE',  ( 0.3410076799406683290, 0.2754140928391118348, 0.1259532371559686781 ) ) ;
#2797 = ADVANCED_FACE ( 'NONE', ( #1256 ), #1087, .T. ) ;
#2798 = CARTESIAN_POINT ( 'NONE',  ( -6.322734125961233610E-17, -0.2702383257424528229, 0.1224846707640861176 ) ) ;
#2799 = EDGE_LOOP ( 'NONE', ( #1249, #2342 ) ) ;
#2800 = CARTESIAN_POINT ( 'NONE',  ( 0.3336175750056032951, -0.2273032555864670234, 0.1968503937007874682 ) ) ;
#2801 = ORIENTED_EDGE ( 'NONE', *, *, #6403, .F. ) ;
#2802 = DIRECTION ( 'NONE',  ( -0.000000000000000000, -0.000000000000000000, 1.000000000000000000 ) ) ;
#2803 = EDGE_LOOP ( 'NONE', ( #3242, #1215, #6993, #4120 ) ) ;
#2804 = DIRECTION ( 'NONE',  ( 0.000000000000000000, 0.000000000000000000, 1.000000000000000000 ) ) ;
#2805 = ADVANCED_FACE ( 'NONE', ( #1292 ), #3637, .T. ) ;
#2806 = ADVANCED_FACE ( 'NONE', ( #1063 ), #1676, .F. ) ;
#2807 = CARTESIAN_POINT ( 'NONE',  ( 25.13671773485889815, 34.81515369617522992, 51.43712309129124094 ) ) ;
#2808 = DIRECTION ( 'NONE',  ( 0.000000000000000000, 0.000000000000000000, -1.000000000000000000 ) ) ;
#2809 = DIRECTION ( 'NONE',  ( -1.000000000000000000, -0.000000000000000000, -0.000000000000000000 ) ) ;
#2810 = CONICAL_SURFACE ( 'NONE', #7441, 0.3543307086614173596, 1.047197551196596521 ) ;
#2811 = ADVANCED_FACE ( 'NONE', ( #967 ), #6949, .T. ) ;
#2812 = CARTESIAN_POINT ( 'NONE',  ( 0.000000000000000000, 1.496062992125984259, 0.000000000000000000 ) ) ;
#2813 = DIRECTION ( 'NONE',  ( -0.000000000000000000, 0.000000000000000000, 1.000000000000000000 ) ) ;
#2814 = DIRECTION ( 'NONE',  ( 0.000000000000000000, 0.000000000000000000, 1.000000000000000000 ) ) ;
#2815 = AXIS2_PLACEMENT_3D ( 'NONE', #1971, #5954, #4186 ) ;
#2816 = DIRECTION ( 'NONE',  ( 0.000000000000000000, 0.000000000000000000, 1.000000000000000000 ) ) ;
#2817 = DIRECTION ( 'NONE',  ( 1.765631543889772066E-46, -1.000000000000000000, -2.207829878515936732E-15 ) ) ;
#2818 = LINE ( 'NONE', #3326, #6249 ) ;
#2819 = AXIS2_PLACEMENT_3D ( 'NONE', #5842, #3506, #7136 ) ;
#2820 = CONTEXT_DEPENDENT_SHAPE_REPRESENTATION ( #1993, #745 ) ;
#2821 = CARTESIAN_POINT ( 'NONE',  ( 0.3581828924050323715, 0.1743168766271107895, -0.3019256869348722061 ) ) ;
#2822 = ORIENTED_EDGE ( 'NONE', *, *, #6180, .F. ) ;
#2823 = CARTESIAN_POINT ( 'NONE',  ( 0.3459463601587655091, 0.3157502742998894996, -0.04365566351111115767 ) ) ;
#2824 = DIRECTION ( 'NONE',  ( 0.000000000000000000, 0.000000000000000000, 1.000000000000000000 ) ) ;
#2825 = AXIS2_PLACEMENT_3D ( 'NONE', #62, #1152, #3581 ) ;
#2826 = AXIS2_PLACEMENT_3D ( 'NONE', #6903, #5037, #6830 ) ;
#2827 = ORIENTED_EDGE ( 'NONE', *, *, #3748, .F. ) ;
#2828 = AXIS2_PLACEMENT_3D ( 'NONE', #1713, #6389, #2897 ) ;
#2829 = VERTEX_POINT ( 'NONE', #1611 ) ;
#2830 = B_SPLINE_CURVE_WITH_KNOTS ( 'NONE', 3,
 ( #3577, #142, #7131, #6034, #3036, #5335, #746, #2998 ),
 .UNSPECIFIED., .F., .F.,
 ( 4, 2, 2, 4 ),
 ( 0.004381617662950684777, 0.005472867551409519790, 0.006564117439868355670, 0.008746617216786024829 ),
 .UNSPECIFIED. ) ;
#2831 = CARTESIAN_POINT ( 'NONE',  ( -0.2073490933073312559, 0.2894328052184277356, 2.399704365528325123E-16 ) ) ;
#2832 = CONICAL_SURFACE ( 'NONE', #7115, 0.4629062255509093782, 1.221730476396037490 ) ;
#2833 = DIRECTION ( 'NONE',  ( -1.000000000000000000, -8.881784197001252323E-16, 0.000000000000000000 ) ) ;
#2834 = ORIENTED_EDGE ( 'NONE', *, *, #7091, .F. ) ;
#2835 = LINE ( 'NONE', #2156, #5232 ) ;
#2836 = EDGE_LOOP ( 'NONE', ( #955, #6067, #5406, #3912 ) ) ;
#2837 = DIRECTION ( 'NONE',  ( -0.000000000000000000, -1.000000000000000000, -0.000000000000000000 ) ) ;
#2838 = ADVANCED_FACE ( 'NONE', ( #5099 ), #6339, .T. ) ;
#2839 = ORIENTED_EDGE ( 'NONE', *, *, #387, .F. ) ;
#2840 = DIRECTION ( 'NONE',  ( -0.000000000000000000, -0.000000000000000000, -1.000000000000000000 ) ) ;
#2841 = LENGTH_MEASURE_WITH_UNIT ( LENGTH_MEASURE( 0.02539999999999999897 ), #4639 );
#2842 = CARTESIAN_POINT ( 'NONE',  ( 0.3561390657006787142, -0.3446602609999988021, 5.012419073868498717E-17 ) ) ;
#2843 = B_SPLINE_CURVE_WITH_KNOTS ( 'NONE', 3,
 ( #500, #2776, #3386, #4467, #2698, #1543 ),
 .UNSPECIFIED., .F., .F.,
 ( 4, 2, 4 ),
 ( 0.01452727543195640389, 0.01715716534226973539, 0.01978705525258306688 ),
 .UNSPECIFIED. ) ;
#2844 = DIRECTION ( 'NONE',  ( -0.000000000000000000, -0.000000000000000000, 1.000000000000000000 ) ) ;
#2845 = CARTESIAN_POINT ( 'NONE',  ( 0.7484094839556201251, 0.01546318525790828929, -0.9841610390795200169 ) ) ;
#2846 = ADVANCED_FACE ( 'NONE', ( #3254, #360 ), #480, .F. ) ;
#2847 = EDGE_CURVE ( 'NONE', #4601, #4341, #5779, .T. ) ;
#2848 = EDGE_CURVE ( 'NONE', #3022, #2114, #4504, .T. ) ;
#2849 = SHAPE_REPRESENTATION_RELATIONSHIP ( 'NONE' , 'NONE' ,  #2147, #3575 ) ;
#2850 = CIRCLE ( 'NONE', #5428, 1.968503937007874072 ) ;
#2851 = PLANE ( 'NONE',  #301 ) ;
#2852 = DIRECTION ( 'NONE',  ( 0.000000000000000000, -0.8660254037844381525, -0.5000000000000009992 ) ) ;
#2853 = CARTESIAN_POINT ( 'NONE',  ( 0.000000000000000000, 0.000000000000000000, -1.546597720061111847 ) ) ;
#2854 = EDGE_CURVE ( 'NONE', #3405, #4833, #3026, .T. ) ;
#2855 = EDGE_CURVE ( 'NONE', #1409, #269, #1031, .T. ) ;
#2856 = TOROIDAL_SURFACE ( 'NONE', #1025, 1.043121362164705745, 0.05905511811023622659 ) ;
#2857 = CARTESIAN_POINT ( 'NONE',  ( 0.9479499796399352141, -0.4353079511162137316, -1.456692913385826849 ) ) ;
#2858 = ITEM_DEFINED_TRANSFORMATION ( 'NONE', 'NONE', #7102,  #5166 ) ;
#2859 = CARTESIAN_POINT ( 'NONE',  ( 0.4685039370078740717, -0.1704774416898505729, -0.2952755905511810774 ) ) ;
#2860 = EDGE_LOOP ( 'NONE', ( #873, #2157, #5250, #1407 ) ) ;
#2861 = CARTESIAN_POINT ( 'NONE',  ( 1.048552902599924730, -0.4330708661417213001, -1.573978973432616835 ) ) ;
#2862 = CARTESIAN_POINT ( 'NONE',  ( 0.3409812221349244332, -0.2467127425962881426, 0.1756638922268692060 ) ) ;
#2863 =( REPRESENTATION_RELATIONSHIP ('NONE','NONE', #303, #7075 ) REPRESENTATION_RELATIONSHIP_WITH_TRANSFORMATION ( #6887 )SHAPE_REPRESENTATION_RELATIONSHIP( ) );
#2864 = VERTEX_POINT ( 'NONE', #1276 ) ;
#2865 = ORIENTED_EDGE ( 'NONE', *, *, #4460, .T. ) ;
#2866 = CARTESIAN_POINT ( 'NONE',  ( -0.2961551751698085488, 0.2381605899494505241, -0.01402797064541873306 ) ) ;
#2867 = CARTESIAN_POINT ( 'NONE',  ( 0.000000000000000000, -0.2557161625347748601, 0.1476377952755911216 ) ) ;
#2868 = ORIENTED_EDGE ( 'NONE', *, *, #3542, .T. ) ;
#2869 = CARTESIAN_POINT ( 'NONE',  ( 1.208238579388023037, 0.07659700195593643901, 0.9813707449069869471 ) ) ;
#2870 = DIRECTION ( 'NONE',  ( 0.000000000000000000, 0.000000000000000000, 1.000000000000000000 ) ) ;
#2871 = ORIENTED_EDGE ( 'NONE', *, *, #1028, .F. ) ;
#2872 = DIRECTION ( 'NONE',  ( 0.000000000000000000, 0.000000000000000000, -1.000000000000000000 ) ) ;
#2873 = DIRECTION ( 'NONE',  ( 1.000000000000000000, 0.000000000000000000, 0.000000000000000000 ) ) ;
#2874 = DIRECTION ( 'NONE',  ( -1.000000000000000000, 0.000000000000000000, 0.000000000000000000 ) ) ;
#2875 = CARTESIAN_POINT ( 'NONE',  ( -0.1621299108466738859, 0.3155401123846230949, -0.4082677165354333115 ) ) ;
#2876 = AXIS2_PLACEMENT_3D ( 'NONE', #86, #4606, #4180 ) ;
#2877 = SURFACE_STYLE_USAGE ( .BOTH. , #6331 ) ;
#2878 = DIRECTION ( 'NONE',  ( 1.000000000000000000, 0.000000000000000000, 0.000000000000000000 ) ) ;
#2879 = EDGE_CURVE ( 'NONE', #4791, #5757, #1444, .T. ) ;
#2880 = CARTESIAN_POINT ( 'NONE',  ( 0.000000000000000000, 0.000000000000000000, 0.000000000000000000 ) ) ;
#2881 = CARTESIAN_POINT ( 'NONE',  ( 2.755905511811024056, 0.000000000000000000, -0.7480314960629921295 ) ) ;
#2882 = CARTESIAN_POINT ( 'NONE',  ( 0.3465697713329959906, -0.1180955399632931530, -0.2952755905511810774 ) ) ;
#2883 = FACE_OUTER_BOUND ( 'NONE', #6810, .T. ) ;
#2884 = CARTESIAN_POINT ( 'NONE',  ( 0.3336175750056032396, 0.2841290694830835850, 0.09842519685039366473 ) ) ;
#2885 = EDGE_CURVE ( 'NONE', #4654, #662, #6694, .T. ) ;
#2886 = ITEM_DEFINED_TRANSFORMATION ( 'NONE', 'NONE', #6308,  #5166 ) ;
#2887 = EDGE_CURVE ( 'NONE', #3371, #4601, #3224, .T. ) ;
#2888 = CARTESIAN_POINT ( 'NONE',  ( -0.4596433552321257388, -0.9990286922241469192, -1.415369843883347967 ) ) ;
#2889 = EDGE_LOOP ( 'NONE', ( #4520, #888, #71, #6177, #3870, #6327 ) ) ;
#2890 = CARTESIAN_POINT ( 'NONE',  ( 1.968503937007874072, 1.496062992125984259, 0.2362204724409449619 ) ) ;
#2891 = EDGE_CURVE ( 'NONE', #4488, #3292, #1578, .T. ) ;
#2892 = DIRECTION ( 'NONE',  ( -0.000000000000000000, -0.000000000000000000, -1.000000000000000000 ) ) ;
#2893 = B_SPLINE_CURVE_WITH_KNOTS ( 'NONE', 3,
 ( #4857, #2073, #7184, #6625, #279, #2600 ),
 .UNSPECIFIED., .F., .F.,
 ( 4, 2, 4 ),
 ( 2.380732026385019675E-07, 0.002190927868076661400, 0.004381617662950684777 ),
 .UNSPECIFIED. ) ;
#2894 = ORIENTED_EDGE ( 'NONE', *, *, #7103, .F. ) ;
#2895 = CIRCLE ( 'NONE', #6440, 0.3543307086614173596 ) ;
#2896 = ORIENTED_EDGE ( 'NONE', *, *, #4347, .F. ) ;
#2897 = DIRECTION ( 'NONE',  ( 1.000000000000000000, 0.000000000000000000, 0.000000000000000000 ) ) ;
#2898 = CARTESIAN_POINT ( 'NONE',  ( 0.000000000000000000, 0.000000000000000000, 0.1188976377952756375 ) ) ;
#2899 = VERTEX_POINT ( 'NONE', #7021 ) ;
#2900 = VECTOR ( 'NONE', #52, 39.37007874015748143 ) ;
#2901 = DIRECTION ( 'NONE',  ( -1.000000000000000000, -0.000000000000000000, -0.000000000000000000 ) ) ;
#2902 = CARTESIAN_POINT ( 'NONE',  ( 0.3485777078273625817, 0.3195689143662219234, -0.04989192643193119531 ) ) ;
#2903 = ORIENTED_EDGE ( 'NONE', *, *, #4615, .T. ) ;
#2904 = ORIENTED_EDGE ( 'NONE', *, *, #4861, .T. ) ;
#2905 = CARTESIAN_POINT ( 'NONE',  ( 0.2699662542182227343, 0.000000000000000000, 0.3732633159281743551 ) ) ;
#2906 = VECTOR ( 'NONE', #1128, 39.37007874015748143 ) ;
#2907 = CARTESIAN_POINT ( 'NONE',  ( 0.3479985092864859020, -0.1192235226163089606, 0.3017044423212984494 ) ) ;
#2908 = CARTESIAN_POINT ( 'NONE',  ( 25.13671773485890526, 34.81515369617522992, 54.18490428891996658 ) ) ;
#2909 = CARTESIAN_POINT ( 'NONE',  ( 0.3411158341578399145, -0.06121148758009550134, 0.3014953708557878698 ) ) ;
#2910 = AXIS2_PLACEMENT_3D ( 'NONE', #4179, #3927, #1539 ) ;
#2911 = CARTESIAN_POINT ( 'NONE',  ( 0.000000000000000000, 0.000000000000000000, -0.4072677165354330331 ) ) ;
#2912 = SHAPE_REPRESENTATION ( 'Supporter', ( #5166 ), #879 ) ;
#2913 = ORIENTED_EDGE ( 'NONE', *, *, #3694, .F. ) ;
#2914 = LENGTH_MEASURE_WITH_UNIT ( LENGTH_MEASURE( 0.02539999999999999897 ), #5804 );
#2915 = CIRCLE ( 'NONE', #3663, 0.1982677165354330695 ) ;
#2916 = CARTESIAN_POINT ( 'NONE',  ( 1.968503937007874072, 0.000000000000000000, 0.000000000000000000 ) ) ;
#2917 = DIRECTION ( 'NONE',  ( -0.000000000000000000, -1.000000000000000000, -0.000000000000000000 ) ) ;
#2918 = LINE ( 'NONE', #5198, #1497 ) ;
#2919 = PRODUCT_RELATED_PRODUCT_CATEGORY ( 'part', '', ( #3614 ) ) ;
#2920 = CARTESIAN_POINT ( 'NONE',  ( -0.1171731013849884873, -0.3414959384292345357, -0.4052515342986934832 ) ) ;
#2921 = DIRECTION ( 'NONE',  ( 0.000000000000000000, 4.632546475182561102E-15, -1.000000000000000000 ) ) ;
#2922 = CARTESIAN_POINT ( 'NONE',  ( -1.048552902599919401, -0.4330708661417353444, -1.573978973432617279 ) ) ;
#2923 = CIRCLE ( 'NONE', #7090, 0.4629062255509093782 ) ;
#2924 = CARTESIAN_POINT ( 'NONE',  ( -0.4637690556582350077, -0.9984401429152556240, -1.410743228759551604 ) ) ;
#2925 = ORIENTED_EDGE ( 'NONE', *, *, #1765, .F. ) ;
#2926 = CARTESIAN_POINT ( 'NONE',  ( 0.3410249605999031153, 0.02920150297965299485, -0.3014927230551893711 ) ) ;
#2927 = CARTESIAN_POINT ( 'NONE',  ( -2.834645669291338432, 0.4724409448818890911, 0.4724409448818902013 ) ) ;
#2928 = EDGE_CURVE ( 'NONE', #5498, #5789, #1818, .T. ) ;
#2929 = EDGE_CURVE ( 'NONE', #2163, #1565, #750, .T. ) ;
#2930 = ORIENTED_EDGE ( 'NONE', *, *, #3645, .T. ) ;
#2931 = CIRCLE ( 'NONE', #3682, 0.2362204724409449341 ) ;
#2932 = VERTEX_POINT ( 'NONE', #7096 ) ;
#2933 = CARTESIAN_POINT ( 'NONE',  ( 1.038078147671274376, -0.2301377692397579833, 0.9569696942589730471 ) ) ;
#2934 = EDGE_CURVE ( 'NONE', #6545, #1603, #2661, .T. ) ;
#2935 = DIRECTION ( 'NONE',  ( -0.000000000000000000, -0.000000000000000000, 1.000000000000000000 ) ) ;
#2936 = ORIENTED_EDGE ( 'NONE', *, *, #6224, .F. ) ;
#2937 = AXIS2_PLACEMENT_3D ( 'NONE', #3925, #5617, #5655 ) ;
#2938 = DIRECTION ( 'NONE',  ( 1.000000000000000000, 0.000000000000000000, 0.000000000000000000 ) ) ;
#2939 = AXIS2_PLACEMENT_3D ( 'NONE', #4868, #3686, #4903 ) ;
#2940 = CARTESIAN_POINT ( 'NONE',  ( -0.9705345056685864558, 0.4659838021920478246, -1.550372027848833545 ) ) ;
#2941 = EDGE_CURVE ( 'NONE', #3522, #75, #5147, .T. ) ;
#2942 = ORIENTED_EDGE ( 'NONE', *, *, #3882, .T. ) ;
#2943 = AXIS2_PLACEMENT_3D ( 'NONE', #6374, #2386, #2350 ) ;
#2944 = DIRECTION ( 'NONE',  ( 2.312579046053608732E-29, -2.207829878515936732E-15, -1.000000000000000000 ) ) ;
#2945 = CARTESIAN_POINT ( 'NONE',  ( 0.000000000000000000, 1.496062992125984259, -0.4921259842519685179 ) ) ;
#2946 = APPLICATION_PROTOCOL_DEFINITION ( 'draft international standard', 'automotive_design', 1998, #3652 ) ;
#2947 = CARTESIAN_POINT ( 'NONE',  ( 0.9842519685039370358, 0.7480314960629921295, 0.000000000000000000 ) ) ;
#2948 = CARTESIAN_POINT ( 'NONE',  ( 0.3543307086614173040, 0.1379824317933222577, -0.3941213672119904809 ) ) ;
#2949 = CARTESIAN_POINT ( 'NONE',  ( 0.2066929133858267931, 0.000000000000000000, -0.4082677165354330340 ) ) ;
#2950 = CARTESIAN_POINT ( 'NONE',  ( -0.4330708661417287941, 0.000000000000000000, -2.204724409448822975 ) ) ;
#2951 = VERTEX_POINT ( 'NONE', #1118 ) ;
#2952 = CIRCLE ( 'NONE', #5670, 1.223643328182682621 ) ;
#2953 = CARTESIAN_POINT ( 'NONE',  ( 0.000000000000000000, 0.000000000000000000, 0.000000000000000000 ) ) ;
#2954 = CARTESIAN_POINT ( 'NONE',  ( 1.968503937007874072, 0.000000000000000000, 0.000000000000000000 ) ) ;
#2955 = ORIENTED_EDGE ( 'NONE', *, *, #6126, .F. ) ;
#2956 = AXIS2_PLACEMENT_3D ( 'NONE', #3662, #6076, #829 ) ;
#2957 = DIRECTION ( 'NONE',  ( 0.000000000000000000, 1.000000000000000000, 0.000000000000000000 ) ) ;
#2958 = FACE_OUTER_BOUND ( 'NONE', #5317, .T. ) ;
#2959 = CARTESIAN_POINT ( 'NONE',  ( 0.4685039370078740717, 0.3409548833797004797, 0.000000000000000000 ) ) ;
#2960 = DIRECTION ( 'NONE',  ( -1.000000000000000000, -0.000000000000000000, -0.000000000000000000 ) ) ;
#2961 = PRODUCT_DEFINITION_CONTEXT ( 'detailed design', #4972, 'design' ) ;
#2962 = LINE ( 'NONE', #3504, #6052 ) ;
#2963 = CARTESIAN_POINT ( 'NONE',  ( 0.9697097892794885876, 0.4330708661417424499, -1.453662943332487023 ) ) ;
#2964 = CARTESIAN_POINT ( 'NONE',  ( -0.9842519685039370358, 1.220472440944881942, 2.480314960629921295 ) ) ;
#2965 = CONTEXT_DEPENDENT_SHAPE_REPRESENTATION ( #1590, #2100 ) ;
#2966 = DIRECTION ( 'NONE',  ( 0.000000000000000000, 0.000000000000000000, 1.000000000000000000 ) ) ;
#2967 = DIRECTION ( 'NONE',  ( 0.000000000000000000, 0.000000000000000000, -1.000000000000000000 ) ) ;
#2968 = CARTESIAN_POINT ( 'NONE',  ( 0.3581828924050324825, -0.1743168766271116221, -0.3019256869348722061 ) ) ;
#2969 = DIRECTION ( 'NONE',  ( 0.000000000000000000, 0.000000000000000000, 1.000000000000000000 ) ) ;
#2970 = ORIENTED_EDGE ( 'NONE', *, *, #4351, .F. ) ;
#2971 = CLOSED_SHELL ( 'NONE', ( #3892, #5725, #1110, #299, #1040, #1809, #6233, #4217, #3273, #1525, #5489, #3220, #937 ) ) ;
#2972 = CARTESIAN_POINT ( 'NONE',  ( -0.4589124540220937964, -1.085572738833920248, -1.540322878613942681 ) ) ;
#2973 = CARTESIAN_POINT ( 'NONE',  ( -0.7480314960629922405, 1.220472440944881942, 2.480314960629921295 ) ) ;
#2974 = ORIENTED_EDGE ( 'NONE', *, *, #245, .T. ) ;
#2975 = ORIENTED_EDGE ( 'NONE', *, *, #287, .F. ) ;
#2976 = AXIS2_PLACEMENT_3D ( 'NONE', #6328, #5152, #2872 ) ;
#2977 = CARTESIAN_POINT ( 'NONE',  ( -1.279527559055117836, 1.968503937007873850, 0.4724409448818898127 ) ) ;
#2978 = EDGE_CURVE ( 'NONE', #7112, #5632, #6711, .T. ) ;
#2979 = CYLINDRICAL_SURFACE ( 'NONE', #3389, 0.4921259842519685179 ) ;
#2980 = ORIENTED_EDGE ( 'NONE', *, *, #613, .F. ) ;
#2981 = CARTESIAN_POINT ( 'NONE',  ( 0.000000000000000000, 0.000000000000000000, 0.000000000000000000 ) ) ;
#2982 = DIRECTION ( 'NONE',  ( -1.000000000000000000, 0.000000000000000000, 0.000000000000000000 ) ) ;
#2983 = ORIENTED_EDGE ( 'NONE', *, *, #4154, .F. ) ;
#2984 = CYLINDRICAL_SURFACE ( 'NONE', #5538, 0.2699662542182227343 ) ;
#2985 = FACE_OUTER_BOUND ( 'NONE', #4226, .T. ) ;
#2986 = DIRECTION ( 'NONE',  ( 0.000000000000000000, 0.000000000000000000, -1.000000000000000000 ) ) ;
#2987 = EDGE_CURVE ( 'NONE', #3423, #4277, #3171, .T. ) ;
#2988 = SURFACE_SIDE_STYLE ('',( #7083 ) ) ;
#2989 = EDGE_CURVE ( 'NONE', #5974, #5274, #7227, .T. ) ;
#2990 = CARTESIAN_POINT ( 'NONE',  ( -1.037563309807726375, 0.4338950423154108171, -1.574803149606299302 ) ) ;
#2991 = ORIENTED_EDGE ( 'NONE', *, *, #3369, .F. ) ;
#2992 = LINE ( 'NONE', #2949, #2068 ) ;
#2993 = DIRECTION ( 'NONE',  ( -4.632546475182562680E-15, 0.000000000000000000, 1.000000000000000000 ) ) ;
#2994 = ORIENTED_EDGE ( 'NONE', *, *, #5635, .F. ) ;
#2995 = CARTESIAN_POINT ( 'NONE',  ( 0.000000000000000000, 1.496062992125984259, 0.000000000000000000 ) ) ;
#2996 = ORIENTED_EDGE ( 'NONE', *, *, #7375, .T. ) ;
#2997 = PRODUCT_DEFINITION_SHAPE ( 'NONE', 'NONE',  #5662 ) ;
#2998 = CARTESIAN_POINT ( 'NONE',  ( 0.02637295201093751290, -0.3409548833797009237, -9.138209691400258722E-18 ) ) ;
#2999 = DIRECTION ( 'NONE',  ( -1.000000000000000000, -0.000000000000000000, -0.000000000000000000 ) ) ;
#3000 = CARTESIAN_POINT ( 'NONE',  ( 0.9842519685039370358, 1.220472440944881942, 2.480314960629921295 ) ) ;
#3001 = LINE ( 'NONE', #679, #2245 ) ;
#3002 = DIRECTION ( 'NONE',  ( 1.047444401652940007E-14, -1.000000000000000000, 0.000000000000000000 ) ) ;
#3003 = FACE_OUTER_BOUND ( 'NONE', #4049, .T. ) ;
#3004 = APPLICATION_CONTEXT ( 'automotive_design' ) ;
#3005 = DIRECTION ( 'NONE',  ( 0.000000000000000000, 0.000000000000000000, -1.000000000000000000 ) ) ;
#3006 = CARTESIAN_POINT ( 'NONE',  ( -0.4596436929058889120, 0.9990286721055804398, -1.415369458146015447 ) ) ;
#3007 = DIRECTION ( 'NONE',  ( 3.491481338843133750E-15, -1.000000000000000000, -0.000000000000000000 ) ) ;
#3008 = CONTEXT_DEPENDENT_SHAPE_REPRESENTATION ( #5121, #6617 ) ;
#3009 = DIRECTION ( 'NONE',  ( 0.000000000000000000, 0.000000000000000000, -1.000000000000000000 ) ) ;
#3010 = CARTESIAN_POINT ( 'NONE',  ( -0.4762522394722485397, -0.9941399105654894486, -1.397361772547375480 ) ) ;
#3011 = ORIENTED_EDGE ( 'NONE', *, *, #7285, .T. ) ;
#3012 = CARTESIAN_POINT ( 'NONE',  ( 0.5141614760841460852, 0.9609181420092316461, -1.361499588670819216 ) ) ;
#3013 = DIRECTION ( 'NONE',  ( 0.000000000000000000, 0.000000000000000000, -1.000000000000000000 ) ) ;
#3014 = ORIENTED_EDGE ( 'NONE', *, *, #3081, .F. ) ;
#3015 = ORIENTED_EDGE ( 'NONE', *, *, #1302, .T. ) ;
#3016 = FACE_BOUND ( 'NONE', #367, .T. ) ;
#3017 = AXIS2_PLACEMENT_3D ( 'NONE', #6911, #2296, #1526 ) ;
#3018 = DIRECTION ( 'NONE',  ( 0.000000000000000000, 0.000000000000000000, 1.000000000000000000 ) ) ;
#3019 = ORIENTED_EDGE ( 'NONE', *, *, #6223, .F. ) ;
#3020 = FACE_OUTER_BOUND ( 'NONE', #1917, .T. ) ;
#3021 = AXIS2_PLACEMENT_3D ( 'NONE', #4773, #5307, #5781 ) ;
#3022 = VERTEX_POINT ( 'NONE', #2248 ) ;
#3023 = ADVANCED_FACE ( 'NONE', ( #2307 ), #3611, .F. ) ;
#3024 = CARTESIAN_POINT ( 'NONE',  ( 0.3411151615605753085, -0.2304996462388200218, -0.2037536041052529223 ) ) ;
#3025 = DIRECTION ( 'NONE',  ( 0.000000000000000000, -0.000000000000000000, 1.000000000000000000 ) ) ;
#3026 = B_SPLINE_CURVE_WITH_KNOTS ( 'NONE', 3,
 ( #6814, #5142, #1568, #3219, #4983, #7301, #6779, #5567, #2081, #3916, #6244, #1003, #3338, #5341, #4196, #6535, #2963, #2353 ),
 .UNSPECIFIED., .F., .F.,
 ( 4, 2, 2, 2, 2, 2, 2, 2, 4 ),
 ( -8.121667112571881724E-06, 0.0009422843086939815564, 0.001417487296597250493, 0.001892690284500519538, 0.002367893272403787715, 0.002843096260307056544, 0.003318299248210325372, 0.003555900742161956316, 0.003793502236113587694 ),
 .UNSPECIFIED. ) ;
#3027 = CONICAL_SURFACE ( 'NONE', #4994, 0.2952755905511810774, 1.047197551196600518 ) ;
#3028 = CARTESIAN_POINT ( 'NONE',  ( 0.01836325778988323956, -0.1427310470019406141, 0.2952755905511810774 ) ) ;
#3029 = B_SPLINE_CURVE_WITH_KNOTS ( 'NONE', 3,
 ( #7361, #2742, #6799, #2626, #1548, #3895 ),
 .UNSPECIFIED., .F., .F.,
 ( 4, 2, 4 ),
 ( -3.269571951033989319E-06, 0.0001651384380483822119, 0.0003335464480477984012 ),
 .UNSPECIFIED. ) ;
#3030 = CARTESIAN_POINT ( 'NONE',  ( 0.4921259842519683514, 0.000000000000000000, -2.204724409448820754 ) ) ;
#3031 = VERTEX_POINT ( 'NONE', #2504 ) ;
#3032 = DIRECTION ( 'NONE',  ( -0.000000000000000000, -1.000000000000000000, -0.000000000000000000 ) ) ;
#3033 = VECTOR ( 'NONE', #7110, 39.37007874015748143 ) ;
#3034 = EDGE_CURVE ( 'NONE', #1896, #7420, #5319, .T. ) ;
#3035 = ADVANCED_FACE ( 'NONE', ( #1985 ), #1808, .T. ) ;
#3036 = CARTESIAN_POINT ( 'NONE',  ( 0.004822332172886453772, -0.2917300191221102734, -0.08525996588982823199 ) ) ;
#3037 = CARTESIAN_POINT ( 'NONE',  ( -1.064268091466843202, 0.5072022184699304104, -1.491294347566136436 ) ) ;
#3038 = AXIS2_PLACEMENT_3D ( 'NONE', #6283, #5025, #4453 ) ;
#3039 = DIRECTION ( 'NONE',  ( 0.000000000000000000, 1.000000000000000000, 0.000000000000000000 ) ) ;
#3040 = CIRCLE ( 'NONE', #3536, 0.2952755905511810774 ) ;
#3041 = PRODUCT_DEFINITION_CONTEXT ( 'detailed design', #1289, 'design' ) ;
#3042 = CARTESIAN_POINT ( 'NONE',  ( -0.4338950423154138147, -1.037563309807725043, -1.574803149606299302 ) ) ;
#3043 = CARTESIAN_POINT ( 'NONE',  ( -0.4843361811957747065, 0.9895437626941984144, -1.389133361342960393 ) ) ;
#3044 = DIRECTION ( 'NONE',  ( 0.000000000000000000, 1.000000000000000000, 0.000000000000000000 ) ) ;
#3045 = CARTESIAN_POINT ( 'NONE',  ( 7.874015748031496287, 0.2559055118110236116, 0.2362204724409455170 ) ) ;
#3046 = CARTESIAN_POINT ( 'NONE',  ( 0.4685039370078740717, 0.3409548833797004797, 0.000000000000000000 ) ) ;
#3047 = DIRECTION ( 'NONE',  ( -1.000000000000000000, 0.000000000000000000, 0.000000000000000000 ) ) ;
#3048 = ORIENTED_EDGE ( 'NONE', *, *, #339, .F. ) ;
#3049 = PRESENTATION_LAYER_ASSIGNMENT (  '', '', ( #5996 ) ) ;
#3050 = CARTESIAN_POINT ( 'NONE',  ( 0.3528822938286762523, 0.1453909600788098055, -0.3018098512751524187 ) ) ;
#3051 = CARTESIAN_POINT ( 'NONE',  ( 0.3410425348215776475, -0.2759054741781712949, 0.1251041708914593653 ) ) ;
#3052 = DIRECTION ( 'NONE',  ( 0.000000000000000000, 0.000000000000000000, 1.000000000000000000 ) ) ;
#3053 = CARTESIAN_POINT ( 'NONE',  ( -1.512058847530491023E-15, 0.4330708661417322913, -2.204724409448820754 ) ) ;
#3054 = DIRECTION ( 'NONE',  ( -1.000000000000000000, -0.000000000000000000, -0.000000000000000000 ) ) ;
#3055 = ORIENTED_EDGE ( 'NONE', *, *, #3739, .F. ) ;
#3056 = CARTESIAN_POINT ( 'NONE',  ( 0.4685039370078740717, 0.1704774416898499345, 0.2952755905511810774 ) ) ;
#3057 = CIRCLE ( 'NONE', #7206, 0.2952755905511810774 ) ;
#3058 = ORIENTED_EDGE ( 'NONE', *, *, #1931, .F. ) ;
#3059 = PRODUCT_DEFINITION_SHAPE ( 'NONE', 'NONE',  #7536 ) ;
#3060 = ORIENTED_EDGE ( 'NONE', *, *, #3262, .F. ) ;
#3061 = CARTESIAN_POINT ( 'NONE',  ( 0.3426144402833997127, -0.2904173629089126796, -0.1000635707556142007 ) ) ;
#3062 = CARTESIAN_POINT ( 'NONE',  ( 0.000000000000000000, 1.496062992125984259, -0.4921259842519685179 ) ) ;
#3063 = PRODUCT_CONTEXT ( 'NONE', #3652, 'mechanical' ) ;
#3064 = AXIS2_PLACEMENT_3D ( 'NONE', #107, #6536, #1277 ) ;
#3065 = CARTESIAN_POINT ( 'NONE',  ( 0.02637295201093707228, -0.1704774416898499345, 0.2952755905511811330 ) ) ;
#3066 = CARTESIAN_POINT ( 'NONE',  ( 0.3565324925542818213, -0.1767206836160838956, 0.2952755905511811885 ) ) ;
#3067 = ORIENTED_EDGE ( 'NONE', *, *, #1542, .T. ) ;
#3068 = AXIS2_PLACEMENT_3D ( 'NONE', #4740, #1831, #2491 ) ;
#3069 = CARTESIAN_POINT ( 'NONE',  ( -1.064268091467049926, -0.5072022184714435333, -1.491294347567520218 ) ) ;
#3070 = EDGE_CURVE ( 'NONE', #2266, #3999, #7069, .T. ) ;
#3071 = CARTESIAN_POINT ( 'NONE',  ( 0.3410425348215776475, -0.2759054741781712949, 0.1251041708914593653 ) ) ;
#3072 =( GEOMETRIC_REPRESENTATION_CONTEXT ( 3 ) GLOBAL_UNCERTAINTY_ASSIGNED_CONTEXT ( ( #3815 ) ) GLOBAL_UNIT_ASSIGNED_CONTEXT ( ( #1664, #6299, #5736 ) ) REPRESENTATION_CONTEXT ( 'NONE', 'WORKASPACE' ) );
#3073 = VERTEX_POINT ( 'NONE', #6045 ) ;
#3074 = LENGTH_MEASURE_WITH_UNIT ( LENGTH_MEASURE( 0.02539999999999999897 ), #2050 );
#3075 = CARTESIAN_POINT ( 'NONE',  ( -0.4663632139997256898, 0.8833361873720764201, -1.436953241411954130 ) ) ;
#3076 = CARTESIAN_POINT ( 'NONE',  ( 0.7480314960629922405, 0.7480314960629921295, 0.000000000000000000 ) ) ;
#3077 = CIRCLE ( 'NONE', #1858, 1.968503937007874072 ) ;
#3078 = ADVANCED_FACE ( 'NONE', ( #6651 ), #155, .T. ) ;
#3079 = ADVANCED_FACE ( 'NONE', ( #3624 ), #1396, .F. ) ;
#3080 = CARTESIAN_POINT ( 'NONE',  ( 3.414809992080329023E-17, 0.4091458600556405201, -0.3766201741223081378 ) ) ;
#3081 = EDGE_CURVE ( 'NONE', #4759, #6192, #3742, .T. ) ;
#3082 = AXIS2_PLACEMENT_3D ( 'NONE', #4701, #6465, #5360 ) ;
#3083 = CARTESIAN_POINT ( 'NONE',  ( 2.892866454678787531E-17, 0.2559055118110236116, 0.2362204724409449341 ) ) ;
#3084 = CARTESIAN_POINT ( 'NONE',  ( 0.4333661275892079501, 1.041228047528454548, -1.574803149606299302 ) ) ;
#3085 = ITEM_DEFINED_TRANSFORMATION ( 'NONE', 'NONE', #2520,  #5166 ) ;
#3086 = CARTESIAN_POINT ( 'NONE',  ( 1.220472440944881942, 0.7480314960629921295, 0.4921259842519685179 ) ) ;
#3087 = DIRECTION ( 'NONE',  ( 0.000000000000000000, -1.000000000000000000, 0.000000000000000000 ) ) ;
#3088 = EDGE_CURVE ( 'NONE', #210, #6925, #4124, .T. ) ;
#3089 = CARTESIAN_POINT ( 'NONE',  ( 0.3581828924050324825, 0.3486337532542225226, 1.056976728655274672E-17 ) ) ;
#3090 = CARTESIAN_POINT ( 'NONE',  ( 0.3543307086614173040, -0.03456946083495027883, -0.4082677165354330895 ) ) ;
#3091 = CARTESIAN_POINT ( 'NONE',  ( 0.000000000000000000, 0.000000000000000000, 0.4921259842519685179 ) ) ;
#3092 = EDGE_CURVE ( 'NONE', #931, #358, #5966, .T. ) ;
#3093 = ORIENTED_EDGE ( 'NONE', *, *, #4961, .T. ) ;
#3094 = CARTESIAN_POINT ( 'NONE',  ( 0.3391892065151629332, -0.1988903486381584651, 0.2460629921259843145 ) ) ;
#3095 = LINE ( 'NONE', #5441, #522 ) ;
#3096 = ORIENTED_EDGE ( 'NONE', *, *, #3938, .F. ) ;
#3097 = AXIS2_PLACEMENT_3D ( 'NONE', #2880, #6406, #3498 ) ;
#3098 = DIRECTION ( 'NONE',  ( 1.000000000000000000, 0.000000000000000000, 0.000000000000000000 ) ) ;
#3099 = ORIENTED_EDGE ( 'NONE', *, *, #245, .F. ) ;
#3100 = CARTESIAN_POINT ( 'NONE',  ( 0.3459463601587655091, 0.3157502742998894996, -0.04365566351111115767 ) ) ;
#3101 = ORIENTED_EDGE ( 'NONE', *, *, #3991, .F. ) ;
#3102 = AXIS2_PLACEMENT_3D ( 'NONE', #5053, #3209, #4475 ) ;
#3103 = EDGE_LOOP ( 'NONE', ( #3996, #5887 ) ) ;
#3104 = CARTESIAN_POINT ( 'NONE',  ( 0.3585569128062319755, -0.1733077889112134284, -0.3036897776982950825 ) ) ;
#3105 = LINE ( 'NONE', #926, #470 ) ;
#3106 = ORIENTED_EDGE ( 'NONE', *, *, #5532, .F. ) ;
#3107 = CARTESIAN_POINT ( 'NONE',  ( 0.3565325103478085289, 0.1673557731150444039, 0.3006824791271354158 ) ) ;
#3108 = ORIENTED_EDGE ( 'NONE', *, *, #5383, .T. ) ;
#3109 =( CONVERSION_BASED_UNIT ( 'INCH', #1342 ) LENGTH_UNIT ( ) NAMED_UNIT ( #1643 ) );
#3110 = DIRECTION ( 'NONE',  ( 0.000000000000000000, 0.000000000000000000, -1.000000000000000000 ) ) ;
#3111 = ORIENTED_EDGE ( 'NONE', *, *, #3794, .T. ) ;
#3112 = CARTESIAN_POINT ( 'NONE',  ( 0.3322361761492684806, -0.2247851515112275766, -0.2012118778978489453 ) ) ;
#3113 = B_SPLINE_CURVE_WITH_KNOTS ( 'NONE', 3,
 ( #147, #6039, #7280, #6110, #1937, #185, #2056, #2584, #4385, #1460 ),
 .UNSPECIFIED., .F., .F.,
 ( 4, 2, 2, 2, 4 ),
 ( -7.765797721861150373E-06, 0.0005114169989440397893, 0.001030599795609940875, 0.001549782592275841852, 0.002068965388941742829 ),
 .UNSPECIFIED. ) ;
#3114 = FILL_AREA_STYLE_COLOUR ( '', #1738 ) ;
#3115 = CARTESIAN_POINT ( 'NONE',  ( 0.3410249605999031153, 0.02920150297965299485, -0.3014927230551893711 ) ) ;
#3116 = UNCERTAINTY_MEASURE_WITH_UNIT (LENGTH_MEASURE( 1.000000000000000082E-05 ), #4344, 'distance_accuracy_value', 'NONE');
#3117 = CARTESIAN_POINT ( 'NONE',  ( 1.279527559055118280, 1.968503937007874072, 2.480314960629921295 ) ) ;
#3118 = EDGE_CURVE ( 'NONE', #7112, #913, #368, .T. ) ;
#3119 = CARTESIAN_POINT ( 'NONE',  ( 21.65354330708661479, 0.000000000000000000, 0.000000000000000000 ) ) ;
#3120 = FACE_OUTER_BOUND ( 'NONE', #2122, .T. ) ;
#3121 = CARTESIAN_POINT ( 'NONE',  ( -2.614463900186501485E-17, 0.02884736746568806673, -0.2952755905511810774 ) ) ;
#3122 = CARTESIAN_POINT ( 'NONE',  ( 0.4338950423154144254, -1.037563309807725043, -1.574803149606299302 ) ) ;
#3123 = DIRECTION ( 'NONE',  ( 0.000000000000000000, 0.000000000000000000, -1.000000000000000000 ) ) ;
#3124 = CARTESIAN_POINT ( 'NONE',  ( 4.923936545553833138E-15, -0.4700904924197903956, -2.204724409448820754 ) ) ;
#3125 = ORIENTED_EDGE ( 'NONE', *, *, #7330, .T. ) ;
#3126 = PRODUCT_DEFINITION_SHAPE ( 'NONE', 'NONE',  #7520 ) ;
#3127 = CARTESIAN_POINT ( 'NONE',  ( 0.1621299108466740524, -0.3155401123846237055, -0.4082677165354329785 ) ) ;
#3128 = CARTESIAN_POINT ( 'NONE',  ( 0.000000000000000000, 0.000000000000000000, -0.3865922971001068409 ) ) ;
#3129 = DIRECTION ( 'NONE',  ( 0.000000000000000000, 0.000000000000000000, 1.000000000000000000 ) ) ;
#3130 = ORIENTED_EDGE ( 'NONE', *, *, #4155, .T. ) ;
#3131 = CARTESIAN_POINT ( 'NONE',  ( 0.3561390657006783811, 0.1723301304999986516, -0.2984845417009731605 ) ) ;
#3132 = ADVANCED_FACE ( 'NONE', ( #7108 ), #1867, .F. ) ;
#3133 = EDGE_CURVE ( 'NONE', #2367, #3143, #796, .T. ) ;
#3134 = FACE_OUTER_BOUND ( 'NONE', #1759, .T. ) ;
#3135 = CARTESIAN_POINT ( 'NONE',  ( -1.048552902599921843, 0.4330708661417285721, -1.573978973432616835 ) ) ;
#3136 = DIRECTION ( 'NONE',  ( 1.000000000000000000, 0.000000000000000000, 0.000000000000000000 ) ) ;
#3137 = EDGE_CURVE ( 'NONE', #4478, #3022, #3491, .T. ) ;
#3138 = CARTESIAN_POINT ( 'NONE',  ( 0.02637295201093703412, 0.1704774416898499345, 0.2952755905511810774 ) ) ;
#3139 = ORIENTED_EDGE ( 'NONE', *, *, #2116, .F. ) ;
#3140 = CARTESIAN_POINT ( 'NONE',  ( 0.3337354549120237213, 0.2261274626982069103, -0.1988869267224314119 ) ) ;
#3141 = EDGE_LOOP ( 'NONE', ( #575, #6671 ) ) ;
#3142 = AXIS2_PLACEMENT_3D ( 'NONE', #2326, #4663, #4283 ) ;
#3143 = VERTEX_POINT ( 'NONE', #4094 ) ;
#3144 = CARTESIAN_POINT ( 'NONE',  ( 0.3321022367506965556, -0.2702568778840481745, -0.1224525375122541698 ) ) ;
#3145 = FILL_AREA_STYLE_COLOUR ( '', #7287 ) ;
#3146 = ORIENTED_EDGE ( 'NONE', *, *, #744, .F. ) ;
#3147 = CARTESIAN_POINT ( 'NONE',  ( -0.2362204724409449619, 2.892866454678788147E-17, -0.9857285720115422922 ) ) ;
#3148 = ORIENTED_EDGE ( 'NONE', *, *, #7505, .T. ) ;
#3149 = CIRCLE ( 'NONE', #4118, 0.3543307086614173596 ) ;
#3150 = CARTESIAN_POINT ( 'NONE',  ( 0.3306743754077733910, -4.012401740694386787E-16, -0.2952755905511810774 ) ) ;
#3151 = ORIENTED_EDGE ( 'NONE', *, *, #7198, .T. ) ;
#3152 = CARTESIAN_POINT ( 'NONE',  ( 1.611653543307086212, 0.000000000000000000, 0.000000000000000000 ) ) ;
#3153 = ORIENTED_EDGE ( 'NONE', *, *, #1626, .F. ) ;
#3154 = VECTOR ( 'NONE', #838, 39.37007874015748143 ) ;
#3155 = LENGTH_MEASURE_WITH_UNIT ( LENGTH_MEASURE( 0.02539999999999999897 ), #1310 );
#3156 = CARTESIAN_POINT ( 'NONE',  ( 0.9842519685039370358, 0.7480314960629921295, 0.000000000000000000 ) ) ;
#3157 =( REPRESENTATION_RELATIONSHIP ('NONE','NONE', #303, #1307 ) REPRESENTATION_RELATIONSHIP_WITH_TRANSFORMATION ( #2455 )SHAPE_REPRESENTATION_RELATIONSHIP( ) );
#3158 = AXIS2_PLACEMENT_3D ( 'NONE', #3670, #4161, #3745 ) ;
#3159 = CARTESIAN_POINT ( 'NONE',  ( 0.4470329974975768006, -1.081428632361001840, -1.553789141944100338 ) ) ;
#3160 = CARTESIAN_POINT ( 'NONE',  ( 1.212519938569362798, 0.06127190455375051276, -0.9823712398279822455 ) ) ;
#3161 = CARTESIAN_POINT ( 'NONE',  ( 0.000000000000000000, 0.2557161625347750267, 0.1476377952755908163 ) ) ;
#3162 = CIRCLE ( 'NONE', #7433, 1.259842519685039353 ) ;
#3163 = CARTESIAN_POINT ( 'NONE',  ( 0.000000000000000000, -0.2557161625347748601, 0.1476377952755911216 ) ) ;
#3164 = DIRECTION ( 'NONE',  ( 0.000000000000000000, 0.000000000000000000, 1.000000000000000000 ) ) ;
#3165 = CARTESIAN_POINT ( 'NONE',  ( -0.2371803407075528947, -0.2722097265016478751, -0.003642820150508878103 ) ) ;
#3166 = DIRECTION ( 'NONE',  ( 0.000000000000000000, 1.000000000000000000, 0.000000000000000000 ) ) ;
#3167 = CARTESIAN_POINT ( 'NONE',  ( -0.3543307086614173040, -0.2045729300278205931, -0.03164754241312491001 ) ) ;
#3168 = ORIENTED_EDGE ( 'NONE', *, *, #6492, .F. ) ;
#3169 = CARTESIAN_POINT ( 'NONE',  ( -0.9983958463931813521, 0.4514963146295044027, -1.424958914991360182 ) ) ;
#3170 = DIRECTION ( 'NONE',  ( 0.000000000000000000, 0.000000000000000000, 1.000000000000000000 ) ) ;
#3171 = CIRCLE ( 'NONE', #2556, 0.9842519685039370358 ) ;
#3172 = ORIENTED_EDGE ( 'NONE', *, *, #3887, .F. ) ;
#3173 = CARTESIAN_POINT ( 'NONE',  ( 0.000000000000000000, 0.000000000000000000, -2.204724409448820754 ) ) ;
#3174 = FACE_OUTER_BOUND ( 'NONE', #6464, .T. ) ;
#3175 = AXIS2_PLACEMENT_3D ( 'NONE', #138, #4300, #6566 ) ;
#3176 = CARTESIAN_POINT ( 'NONE',  ( 0.01178921041716320811, 0.1149842948508782436, 0.2952755905511810774 ) ) ;
#3177 = ORIENTED_EDGE ( 'NONE', *, *, #7514, .T. ) ;
#3178 = CARTESIAN_POINT ( 'NONE',  ( 0.3487102105009307618, 0.2024297391849447236, -0.2527898980517343519 ) ) ;
#3179 = B_SPLINE_CURVE_WITH_KNOTS ( 'NONE', 3,
 ( #6918, #3985, #6311, #2113, #4013, #6344, #3440, #6952, #4653, #2888, #2924, #3508, #3010, #1706, #5346, #2286, #2395, #4048 ),
 .UNSPECIFIED., .F., .F.,
 ( 4, 2, 2, 2, 2, 2, 2, 2, 4 ),
 ( 0.000000000000000000, 0.0002385177155853689210, 0.0004770354311707378421, 0.0009540708623414871766, 0.001431106293512236349, 0.001908141724682985629, 0.002385177155853734909, 0.002862212587024484407, 0.003816283449365995978 ),
 .UNSPECIFIED. ) ;
#3180 = ADVANCED_FACE ( 'NONE', ( #5860 ), #3521, .T. ) ;
#3181 = ADVANCED_FACE ( 'NONE', ( #4062 ), #6393, .T. ) ;
#3182 = EDGE_LOOP ( 'NONE', ( #5362, #1070, #475, #2084 ) ) ;
#3183 = EDGE_LOOP ( 'NONE', ( #2127, #7269 ) ) ;
#3184 = EDGE_CURVE ( 'NONE', #1691, #709, #4862, .T. ) ;
#3185 = DIRECTION ( 'NONE',  ( 0.000000000000000000, 0.000000000000000000, 1.000000000000000000 ) ) ;
#3186 = DIRECTION ( 'NONE',  ( -1.047444401652940007E-14, 1.000000000000000000, -4.625929269271482167E-15 ) ) ;
#3187 = ORIENTED_EDGE ( 'NONE', *, *, #4305, .F. ) ;
#3188 = AXIS2_PLACEMENT_3D ( 'NONE', #3152, #3693, #708 ) ;
#3189 = CARTESIAN_POINT ( 'NONE',  ( 0.7480314960629923515, 1.544184662414706467E-22, 0.9842519685039370358 ) ) ;
#3190 = ORIENTED_EDGE ( 'NONE', *, *, #701, .F. ) ;
#3191 = ADVANCED_FACE ( 'NONE', ( #1107 ), #1752, .F. ) ;
#3192 = DIRECTION ( 'NONE',  ( -1.000000000000000000, -0.000000000000000000, -0.000000000000000000 ) ) ;
#3193 = ORIENTED_EDGE ( 'NONE', *, *, #4676, .T. ) ;
#3194 = B_SPLINE_CURVE_WITH_KNOTS ( 'NONE', 3,
 ( #5859, #1254, #4666, #620, #697, #5279 ),
 .UNSPECIFIED., .F., .F.,
 ( 4, 2, 4 ),
 ( 0.000000000000000000, 0.002233368740102889029, 0.004466737480205778058 ),
 .UNSPECIFIED. ) ;
#3195 = PRODUCT_DEFINITION_SHAPE ( 'NONE', 'NONE',  #2745 ) ;
#3196 = DIRECTION ( 'NONE',  ( 0.000000000000000000, 1.000000000000000000, 0.000000000000000000 ) ) ;
#3197 = CARTESIAN_POINT ( 'NONE',  ( 1.218929327210600766, -0.03110856596261698734, -0.9838783093560928839 ) ) ;
#3198 = CIRCLE ( 'NONE', #4171, 1.124634398195722973 ) ;
#3199 = CARTESIAN_POINT ( 'NONE',  ( 0.000000000000000000, 1.496062992125984259, 0.4921259842519685179 ) ) ;
#3200 = B_SPLINE_CURVE_WITH_KNOTS ( 'NONE', 3,
 ( #2519, #6619, #788, #100, #1806, #4838, #7052, #1936, #3075, #4266 ),
 .UNSPECIFIED., .F., .F.,
 ( 4, 2, 2, 2, 4 ),
 ( 0.000000000000000000, 0.0005216184974661253193, 0.001043236994932250639, 0.001564855492398375958, 0.002086473989864501277 ),
 .UNSPECIFIED. ) ;
#3201 = DIRECTION ( 'NONE',  ( 0.000000000000000000, 0.000000000000000000, -1.000000000000000000 ) ) ;
#3202 = TOROIDAL_SURFACE ( 'NONE', #6023, 0.2948818897637794367, 0.05944881889763781874 ) ;
#3203 = CARTESIAN_POINT ( 'NONE',  ( 0.000000000000000000, 0.000000000000000000, -0.7480314960629921295 ) ) ;
#3204 = CARTESIAN_POINT ( 'NONE',  ( 0.3483227611829846637, -0.1704774416898499345, 0.2952755905511811330 ) ) ;
#3205 = EDGE_LOOP ( 'NONE', ( #3372, #4901, #6666, #4458, #6635, #6524 ) ) ;
#3206 = CARTESIAN_POINT ( 'NONE',  ( -0.3543307086614173040, 0.2045729300278199547, -0.4082677165354330340 ) ) ;
#3207 = CARTESIAN_POINT ( 'NONE',  ( 0.3253487914207032761, -0.2213056477483782147, -0.3862808132025620234 ) ) ;
#3208 = CIRCLE ( 'NONE', #1120, 1.223643328182681511 ) ;
#3209 = DIRECTION ( 'NONE',  ( -0.000000000000000000, 1.000000000000000000, 1.224646799147353207E-16 ) ) ;
#3210 = CARTESIAN_POINT ( 'NONE',  ( 7.874015748031496287, 0.000000000000000000, -0.4921259842519685179 ) ) ;
#3211 = CARTESIAN_POINT ( 'NONE',  ( 0.01832242175888456129, 0.3270109559553079359, -0.02415159075610075201 ) ) ;
#3212 = CARTESIAN_POINT ( 'NONE',  ( 0.4630671888207407161, 1.085749034841581695, -1.535808138920397026 ) ) ;
#3213 = EDGE_LOOP ( 'NONE', ( #2601, #1826, #3612, #6502, #406, #6241 ) ) ;
#3214 = CARTESIAN_POINT ( 'NONE',  ( -0.9479499796399322165, 0.4353079511162203374, -1.456692913385826849 ) ) ;
#3215 =( BOUNDED_SURFACE ( )  B_SPLINE_SURFACE ( 3, 2, ( 
 ( #4623, #2224, #4016 ),
 ( #5784, #393, #6922 ),
 ( #5679, #6240, #437 ),
 ( #1679, #3368, #2862 ),
 ( #5095, #7412, #6891 ),
 ( #5205, #2185, #3988 ),
 ( #4519, #2720, #1037 ),
 ( #6348, #1605, #2791 ) ),
 .UNSPECIFIED., .F., .F., .F. ) 
 B_SPLINE_SURFACE_WITH_KNOTS ( ( 4, 2, 2, 4 ),
 ( 3, 3 ),
 ( 0.03551798592901338203, 0.03994769179990646790, 0.04216254473535301084, 0.04437739767079956071 ),
 ( 0.000000000000000000, 1.000000000000000000 ),
 .UNSPECIFIED. ) 
 GEOMETRIC_REPRESENTATION_ITEM ( )  RATIONAL_B_SPLINE_SURFACE ( (
 ( 1.000000000000000000, 0.8047781103519389134, 1.000000000000000000),
 ( 1.000000000000000000, 0.8123785826170312196, 1.000000000000000000),
 ( 1.000000000000000000, 0.8190671539034724002, 1.000000000000000000),
 ( 1.000000000000000000, 0.8191932076449992550, 1.000000000000000000),
 ( 1.000000000000000000, 0.8176085094069774906, 1.000000000000000000),
 ( 1.000000000000000000, 0.8122955484010631055, 1.000000000000000000),
 ( 1.000000000000000000, 0.8086308001283356583, 1.000000000000000000),
 ( 1.000000000000000000, 0.8047712537969732294, 1.000000000000000000) ) ) 
 REPRESENTATION_ITEM ( '' )  SURFACE ( )  );
#3216 = EDGE_LOOP ( 'NONE', ( #5206, #7195, #6820, #4849 ) ) ;
#3217 = ORIENTED_EDGE ( 'NONE', *, *, #661, .T. ) ;
#3218 = CARTESIAN_POINT ( 'NONE',  ( 0.003035684155427393477, -0.2845908893795038308, -0.09762530132584867903 ) ) ;
#3219 = CARTESIAN_POINT ( 'NONE',  ( 0.9867934559254182281, 0.4882980771758929639, -1.385219299502222556 ) ) ;
#3220 = ADVANCED_FACE ( 'NONE', ( #6426 ), #4634, .F. ) ;
#3221 = CARTESIAN_POINT ( 'NONE',  ( 0.2961551751698085488, -0.2381605899494510792, -0.01402797064541896205 ) ) ;
#3222 = CARTESIAN_POINT ( 'NONE',  ( -0.02898191724071497513, -0.3924131423350826764, -0.02198690333287099327 ) ) ;
#3223 = EDGE_LOOP ( 'NONE', ( #258, #2827 ) ) ;
#3224 = B_SPLINE_CURVE_WITH_KNOTS ( 'NONE', 3,
 ( #4812, #65, #5880, #642, #3043, #4727, #2476, #5305, #3006, #2391, #5385, #1774, #1157, #106, #3585, #3505, #5841, #4768 ),
 .UNSPECIFIED., .F., .F.,
 ( 4, 2, 2, 2, 2, 2, 2, 2, 4 ),
 ( -8.121667112564153395E-06, 0.0009422843086939946752, 0.001417487296597265889, 0.001892690284500537319, 0.002367893272403808966, 0.002843096260307079962, 0.003318299248210351392, 0.003555900742161983638, 0.003793502236113614583 ),
 .UNSPECIFIED. ) ;
#3225 = DIRECTION ( 'NONE',  ( -0.000000000000000000, -0.000000000000000000, 1.000000000000000000 ) ) ;
#3226 = ORIENTED_EDGE ( 'NONE', *, *, #2887, .T. ) ;
#3227 = CLOSED_SHELL ( 'NONE', ( #7427, #751, #1814, #6827, #3361, #3023, #4755, #3079, #6141, #4917 ) ) ;
#3228 =( CONVERSION_BASED_UNIT ( 'INCH', #7310 ) LENGTH_UNIT ( ) NAMED_UNIT ( #2239 ) );
#3229 = ORIENTED_EDGE ( 'NONE', *, *, #5325, .T. ) ;
#3230 = ORIENTED_EDGE ( 'NONE', *, *, #1115, .T. ) ;
#3231 = EDGE_CURVE ( 'NONE', #4290, #2380, #2369, .T. ) ;
#3232 = EDGE_CURVE ( 'NONE', #4990, #1208, #4132, .T. ) ;
#3233 = DIRECTION ( 'NONE',  ( 1.000000000000000000, 0.000000000000000000, 0.000000000000000000 ) ) ;
#3234 = DIRECTION ( 'NONE',  ( -0.000000000000000000, -1.000000000000000000, -0.000000000000000000 ) ) ;
#3235 = DIRECTION ( 'NONE',  ( -1.000000000000000000, -0.000000000000000000, -0.000000000000000000 ) ) ;
#3236 = DIRECTION ( 'NONE',  ( -0.000000000000000000, -0.000000000000000000, 1.000000000000000000 ) ) ;
#3237 = CARTESIAN_POINT ( 'NONE',  ( 0.3483227611829849413, -0.3409548833797009237, 0.000000000000000000 ) ) ;
#3238 = CARTESIAN_POINT ( 'NONE',  ( 1.968503937007874072, 1.205361022782827973E-16, -0.9842519685039370358 ) ) ;
#3239 = CARTESIAN_POINT ( 'NONE',  ( 0.9044344578135206092, -0.4526814320286376425, -1.447629106959917200 ) ) ;
#3240 = CARTESIAN_POINT ( 'NONE',  ( 0.3337354549120238878, -0.2261274626982048841, 0.1988869267224354920 ) ) ;
#3241 = DIRECTION ( 'NONE',  ( 0.000000000000000000, 0.000000000000000000, -1.000000000000000000 ) ) ;
#3242 = ORIENTED_EDGE ( 'NONE', *, *, #3416, .F. ) ;
#3243 = DIRECTION ( 'NONE',  ( 1.000000000000000000, 0.000000000000000000, 0.000000000000000000 ) ) ;
#3244 = DIRECTION ( 'NONE',  ( -1.000000000000000000, -0.000000000000000000, -0.000000000000000000 ) ) ;
#3245 = CARTESIAN_POINT ( 'NONE',  ( 0.3388530074223801147, 0.06137376066181338130, -0.2952755905511810774 ) ) ;
#3246 = CARTESIAN_POINT ( 'NONE',  ( 0.4878048847236821084, 1.078368654584403785, -1.510181419419387439 ) ) ;
#3247 = VERTEX_POINT ( 'NONE', #1214 ) ;
#3248 = PRODUCT_DEFINITION_FORMATION_WITH_SPECIFIED_SOURCE ( 'ANY', '', #1216, .NOT_KNOWN. ) ;
#3249 = DIRECTION ( 'NONE',  ( -0.000000000000000000, -1.000000000000000000, -0.000000000000000000 ) ) ;
#3250 = ORIENTED_EDGE ( 'NONE', *, *, #2855, .F. ) ;
#3251 = PRODUCT_DEFINITION_SHAPE ( 'NONE', 'NONE',  #7534 ) ;
#3252 = VERTEX_POINT ( 'NONE', #3562 ) ;
#3253 = CARTESIAN_POINT ( 'NONE',  ( 1.037563309807720380, 0.4338950423154246394, -1.574803149606299302 ) ) ;
#3254 = FACE_BOUND ( 'NONE', #3103, .T. ) ;
#3255 = APPLICATION_CONTEXT ( 'automotive_design' ) ;
#3256 = DIRECTION ( 'NONE',  ( -1.000000000000000000, -0.000000000000000000, -0.000000000000000000 ) ) ;
#3257 = ORIENTED_EDGE ( 'NONE', *, *, #7283, .F. ) ;
#3258 = CARTESIAN_POINT ( 'NONE',  ( 0.9773775067402716843, -0.4999746636856364779, -1.373988502838978665 ) ) ;
#3259 = ORIENTED_EDGE ( 'NONE', *, *, #7229, .T. ) ;
#3260 = CARTESIAN_POINT ( 'NONE',  ( 1.060520566440911416, 0.2241008867759824719, 0.9584192624488059309 ) ) ;
#3261 = CARTESIAN_POINT ( 'NONE',  ( 0.3426144402834028768, 0.2904173629089201736, 0.1000635707556194326 ) ) ;
#3262 = EDGE_CURVE ( 'NONE', #4878, #2461, #4038, .T. ) ;
#3263 = EDGE_LOOP ( 'NONE', ( #37, #4627 ) ) ;
#3264 = VERTEX_POINT ( 'NONE', #3878 ) ;
#3265 = DIRECTION ( 'NONE',  ( -1.000000000000000000, 0.000000000000000000, 0.000000000000000000 ) ) ;
#3266 = CARTESIAN_POINT ( 'NONE',  ( 1.968503937007874072, 1.496062992125984259, 0.4921259842519685179 ) ) ;
#3267 = DIRECTION ( 'NONE',  ( -1.000000000000000000, -0.000000000000000000, -0.000000000000000000 ) ) ;
#3268 = CARTESIAN_POINT ( 'NONE',  ( 1.189145543181157505, -0.1185714375127665254, -0.9771702786582192601 ) ) ;
#3269 = DIRECTION ( 'NONE',  ( 0.000000000000000000, 0.000000000000000000, 1.000000000000000000 ) ) ;
#3270 = EDGE_CURVE ( 'NONE', #1565, #1607, #5188, .T. ) ;
#3271 = EDGE_CURVE ( 'NONE', #5720, #269, #938, .T. ) ;
#3272 = CIRCLE ( 'NONE', #476, 1.043121362164705745 ) ;
#3273 = ADVANCED_FACE ( 'NONE', ( #5414 ), #625, .F. ) ;
#3274 = CARTESIAN_POINT ( 'NONE',  ( 0.4466261709646375810, 0.9159932075028739407, -1.451746187131333521 ) ) ;
#3275 = AXIS2_PLACEMENT_3D ( 'NONE', #3030, #4223, #6561 ) ;
#3276 = DIRECTION ( 'NONE',  ( 1.000000000000000000, 0.000000000000000000, 0.000000000000000000 ) ) ;
#3277 = CARTESIAN_POINT ( 'NONE',  ( 1.010074371201537424, -0.4416272204090869735, -1.570717485485533249 ) ) ;
#3278 = CARTESIAN_POINT ( 'NONE',  ( -0.7480314960629922405, 1.220472440944881942, 0.4724409448818898127 ) ) ;
#3279 = CARTESIAN_POINT ( 'NONE',  ( 0.1470270249832138498, -0.3242597676034328358, -0.4075196867561205472 ) ) ;
#3280 = EDGE_CURVE ( 'NONE', #161, #4527, #2339, .T. ) ;
#3281 = EDGE_LOOP ( 'NONE', ( #446, #3628, #7452, #3096, #6663 ) ) ;
#3282 = VECTOR ( 'NONE', #5308, 39.37007874015748143 ) ;
#3283 = DIRECTION ( 'NONE',  ( 0.000000000000000000, 0.000000000000000000, 1.000000000000000000 ) ) ;
#3284 = CARTESIAN_POINT ( 'NONE',  ( 0.3426404862726872280, -0.2318193597401798645, -0.2015595396344879719 ) ) ;
#3285 = SHAPE_DEFINITION_REPRESENTATION ( #4778, #2104 ) ;
#3286 = CARTESIAN_POINT ( 'NONE',  ( 0.1922007978147438345, 0.2981786776988372134, 2.535346354227414414E-16 ) ) ;
#3287 = ORIENTED_EDGE ( 'NONE', *, *, #3427, .F. ) ;
#3288 = DIRECTION ( 'NONE',  ( 1.000000000000000000, 0.000000000000000000, 0.000000000000000000 ) ) ;
#3289 = VECTOR ( 'NONE', #1139, 39.37007874015748143 ) ;
#3290 = LINE ( 'NONE', #962, #2473 ) ;
#3291 = EDGE_LOOP ( 'NONE', ( #2001, #3377, #1365, #4416 ) ) ;
#3292 = VERTEX_POINT ( 'NONE', #666 ) ;
#3293 = CARTESIAN_POINT ( 'NONE',  ( 0.01165389088406399223, -0.1143408654217484000, -0.2952755905511810219 ) ) ;
#3294 = AXIS2_PLACEMENT_3D ( 'NONE', #3156, #864, #6148 ) ;
#3295 = DIRECTION ( 'NONE',  ( 0.000000000000000000, 1.000000000000000000, 0.000000000000000000 ) ) ;
#3296 = ORIENTED_EDGE ( 'NONE', *, *, #1077, .F. ) ;
#3297 = CARTESIAN_POINT ( 'NONE',  ( 1.850393700787401619, 0.7480314960629921295, -0.7480314960629921295 ) ) ;
#3298 = EDGE_LOOP ( 'NONE', ( #6286, #6214, #2593 ) ) ;
#3299 = CARTESIAN_POINT ( 'NONE',  ( 1.089019577240956993, 0.2122777770860161672, 0.9611070884360988220 ) ) ;
#3300 = ORIENTED_EDGE ( 'NONE', *, *, #4904, .F. ) ;
#3301 = CARTESIAN_POINT ( 'NONE',  ( 0.4330708661417322913, -0.9666437042230126009, -1.454455828411335583 ) ) ;
#3302 = ORIENTED_EDGE ( 'NONE', *, *, #5061, .F. ) ;
#3303 = CARTESIAN_POINT ( 'NONE',  ( -2.614463900186501485E-17, 0.02884736746568806673, -0.2952755905511810774 ) ) ;
#3304 = B_SPLINE_CURVE_WITH_KNOTS ( 'NONE', 3,
 ( #1700, #2349, #1055, #5194, #4005, #3973 ),
 .UNSPECIFIED., .F., .F.,
 ( 4, 2, 4 ),
 ( 0.01452727543195640389, 0.01715716534226972845, 0.01978705525258304954 ),
 .UNSPECIFIED. ) ;
#3305 = DIRECTION ( 'NONE',  ( 1.000000000000000000, 0.000000000000000000, 0.000000000000000000 ) ) ;
#3306 = AXIS2_PLACEMENT_3D ( 'NONE', #5851, #5273, #2489 ) ;
#3307 = CARTESIAN_POINT ( 'NONE',  ( 0.000000000000000000, 0.000000000000000000, 0.4921259842519685179 ) ) ;
#3308 = PRODUCT_RELATED_PRODUCT_CATEGORY ( 'part', '', ( #5591 ) ) ;
#3309 = CARTESIAN_POINT ( 'NONE',  ( 0.000000000000000000, 2.957312202238506242E-17, 0.2952755905511810774 ) ) ;
#3310 = FILL_AREA_STYLE ('',( #906 ) ) ;
#3311 = B_SPLINE_CURVE_WITH_KNOTS ( 'NONE', 3,
 ( #6838, #3894, #6187, #1546, #6225, #3431, #5045, #3314, #5663, #3353 ),
 .UNSPECIFIED., .F., .F.,
 ( 4, 2, 2, 2, 4 ),
 ( 0.000000000000000000, 0.0005494620090385933520, 0.001098924018077186704, 0.001648386027115780056, 0.002197848036154373408 ),
 .UNSPECIFIED. ) ;
#3312 = DIRECTION ( 'NONE',  ( 0.000000000000000000, 0.000000000000000000, 1.000000000000000000 ) ) ;
#3313 = AXIS2_PLACEMENT_3D ( 'NONE', #3119, #5466, #5586 ) ;
#3314 = CARTESIAN_POINT ( 'NONE',  ( 0.4619485889667626077, 0.9755734897585890408, -1.553989674004692567 ) ) ;
#3315 = EDGE_CURVE ( 'NONE', #443, #4433, #4268, .T. ) ;
#3316 = EDGE_CURVE ( 'NONE', #1, #5128, #4022, .T. ) ;
#3317 = DIRECTION ( 'NONE',  ( -7.708596820178695308E-30, 2.207829878515936732E-15, -1.000000000000000000 ) ) ;
#3318 = CARTESIAN_POINT ( 'NONE',  ( 0.3410249605999410294, 1.062103031354818709E-12, 0.3014927230551906479 ) ) ;
#3319 = DIRECTION ( 'NONE',  ( -1.000000000000000000, 0.000000000000000000, 0.000000000000000000 ) ) ;
#3320 = CARTESIAN_POINT ( 'NONE',  ( 0.002479217192759452203, -0.05744896992506681732, 0.2952755905511810774 ) ) ;
#3321 = EDGE_CURVE ( 'NONE', #6553, #1, #4596, .T. ) ;
#3322 = AXIS2_PLACEMENT_3D ( 'NONE', #3430, #672, #7088 ) ;
#3323 = VERTEX_POINT ( 'NONE', #1756 ) ;
#3324 = AXIS2_PLACEMENT_3D ( 'NONE', #6487, #1701, #3469 ) ;
#3325 = CYLINDRICAL_SURFACE ( 'NONE', #1747, 0.2362204724409449341 ) ;
#3326 = CARTESIAN_POINT ( 'NONE',  ( 0.5118110236220474452, 1.220472440944881942, 0.4724409448818898127 ) ) ;
#3327 = ADVANCED_FACE ( 'NONE', ( #2985 ), #3964, .F. ) ;
#3328 = ITEM_DEFINED_TRANSFORMATION ( 'NONE', 'NONE', #78,  #5166 ) ;
#3329 = EDGE_CURVE ( 'NONE', #5818, #1513, #5245, .T. ) ;
#3330 = CARTESIAN_POINT ( 'NONE',  ( -0.9609181420092316461, -0.5141614760841496379, -1.361499588670821659 ) ) ;
#3331 = VERTEX_POINT ( 'NONE', #2052 ) ;
#3332 = CARTESIAN_POINT ( 'NONE',  ( 0.3409812221349237671, 0.2467127425963012433, -0.1756638922268426994 ) ) ;
#3333 = DIRECTION ( 'NONE',  ( 0.000000000000000000, 0.000000000000000000, 1.000000000000000000 ) ) ;
#3334 = EDGE_LOOP ( 'NONE', ( #4670, #6789, #195, #6417 ) ) ;
#3335 = EDGE_LOOP ( 'NONE', ( #5494, #2642, #4330, #6989, #987, #654 ) ) ;
#3336 = AXIS2_PLACEMENT_3D ( 'NONE', #2205, #1017, #2247 ) ;
#3337 = DIRECTION ( 'NONE',  ( -3.491481338843133750E-15, 1.000000000000000000, 0.000000000000000000 ) ) ;
#3338 = CARTESIAN_POINT ( 'NONE',  ( 0.9883301303667288984, 0.4377665650305739842, -1.443420399700356072 ) ) ;
#3339 = ORIENTED_EDGE ( 'NONE', *, *, #1439, .F. ) ;
#3340 = CARTESIAN_POINT ( 'NONE',  ( 2.755905511811024056, 1.496062992125984259, 0.7480314960629921295 ) ) ;
#3341 = ORIENTED_EDGE ( 'NONE', *, *, #6825, .T. ) ;
#3342 = CARTESIAN_POINT ( 'NONE',  ( 0.000000000000000000, 0.000000000000000000, -0.9857285720115422922 ) ) ;
#3343 = FILL_AREA_STYLE_COLOUR ( '', #6607 ) ;
#3344 = ORIENTED_EDGE ( 'NONE', *, *, #2155, .T. ) ;
#3345 = VECTOR ( 'NONE', #4542, 39.37007874015748143 ) ;
#3346 = VERTEX_POINT ( 'NONE', #3307 ) ;
#3347 = CARTESIAN_POINT ( 'NONE',  ( 33.89456220084339577, 40.86510553864606266, 54.38594198892902654 ) ) ;
#3348 = CARTESIAN_POINT ( 'NONE',  ( 0.2362204724409449341, 0.000000000000000000, -0.7983802283864780414 ) ) ;
#3349 = CARTESIAN_POINT ( 'NONE',  ( -1.781909941321919274E-15, 0.000000000000000000, -1.397637795275591843 ) ) ;
#3350 = PLANE ( 'NONE',  #7463 ) ;
#3351 = CARTESIAN_POINT ( 'NONE',  ( 1.038078147671274376, 0.2301377692397579833, -0.9569696942589730471 ) ) ;
#3352 = AXIS2_PLACEMENT_3D ( 'NONE', #4672, #7499, #5190 ) ;
#3353 = CARTESIAN_POINT ( 'NONE',  ( 0.4700904924197906176, 0.9659644734970541657, -1.546597720061111847 ) ) ;
#3354 = DIMENSIONAL_EXPONENTS ( 1.000000000000000000, 0.000000000000000000, 0.000000000000000000, 0.000000000000000000, 0.000000000000000000, 0.000000000000000000, 0.000000000000000000 ) ;
#3355 = DIRECTION ( 'NONE',  ( 1.000000000000000000, 0.000000000000000000, 0.000000000000000000 ) ) ;
#3356 = FACE_OUTER_BOUND ( 'NONE', #364, .T. ) ;
#3357 = CARTESIAN_POINT ( 'NONE',  ( 0.000000000000000000, 0.000000000000000000, 0.000000000000000000 ) ) ;
#3358 = ORIENTED_EDGE ( 'NONE', *, *, #7320, .T. ) ;
#3359 = UNCERTAINTY_MEASURE_WITH_UNIT (LENGTH_MEASURE( 1.000000000000000082E-05 ), #1271, 'distance_accuracy_value', 'NONE');
#3360 = PLANE ( 'NONE',  #2487 ) ;
#3361 = ADVANCED_FACE ( 'NONE', ( #335 ), #904, .T. ) ;
#3362 = VERTEX_POINT ( 'NONE', #3886 ) ;
#3363 = CARTESIAN_POINT ( 'NONE',  ( 0.3997746709170348356, 0.000000000000000000, 0.000000000000000000 ) ) ;
#3364 = FACE_OUTER_BOUND ( 'NONE', #2799, .T. ) ;
#3365 = CARTESIAN_POINT ( 'NONE',  ( 0.2520187439128737106, 0.2636427704167112473, -0.005786797686151470485 ) ) ;
#3366 = VERTEX_POINT ( 'NONE', #3348 ) ;
#3367 = DIRECTION ( 'NONE',  ( 1.000000000000000000, 0.000000000000000000, -0.000000000000000000 ) ) ;
#3368 = CARTESIAN_POINT ( 'NONE',  ( 0.3387177083556423551, -0.2412911239081454440, 0.1726226950780508362 ) ) ;
#3369 = EDGE_CURVE ( 'NONE', #489, #3323, #6831, .T. ) ;
#3370 = EDGE_CURVE ( 'NONE', #4133, #4166, #2736, .T. ) ;
#3371 = VERTEX_POINT ( 'NONE', #5579 ) ;
#3372 = ORIENTED_EDGE ( 'NONE', *, *, #4289, .F. ) ;
#3373 = CARTESIAN_POINT ( 'NONE',  ( 0.9688787811271879491, -0.2362268424322147564, 0.9554835511204313736 ) ) ;
#3374 = DIRECTION ( 'NONE',  ( 1.000000000000000000, 0.000000000000000000, 2.207829878515936732E-15 ) ) ;
#3375 = EDGE_CURVE ( 'NONE', #6858, #7488, #2915, .T. ) ;
#3376 = PRESENTATION_STYLE_ASSIGNMENT (( #4524 ) ) ;
#3377 = ORIENTED_EDGE ( 'NONE', *, *, #4216, .F. ) ;
#3378 = FACE_OUTER_BOUND ( 'NONE', #3861, .T. ) ;
#3379 = ORIENTED_EDGE ( 'NONE', *, *, #4067, .T. ) ;
#3380 = CARTESIAN_POINT ( 'NONE',  ( 1.128157436560226712, 0.1874853199515785218, 0.9662432197917761867 ) ) ;
#3381 = ORIENTED_EDGE ( 'NONE', *, *, #4662, .F. ) ;
#3382 = CIRCLE ( 'NONE', #6220, 0.3543307086614172485 ) ;
#3383 = LINE ( 'NONE', #7392, #6656 ) ;
#3384 = DIRECTION ( 'NONE',  ( -0.4724509005743148249, 0.8813569915457180048, 1.194765668411096211E-16 ) ) ;
#3385 = DIRECTION ( 'NONE',  ( 0.000000000000000000, 0.000000000000000000, 1.000000000000000000 ) ) ;
#3386 = CARTESIAN_POINT ( 'NONE',  ( -0.3543307086614173040, 0.06965032677943208683, -0.4052140698951960385 ) ) ;
#3387 = CARTESIAN_POINT ( 'NONE',  ( 0.9080621969490132450, 0.2241341580870719608, -0.9584117186519856002 ) ) ;
#3388 = B_SPLINE_CURVE_WITH_KNOTS ( 'NONE', 3,
 ( #6912, #5671, #567, #2785, #7443, #1672, #2178, #4009, #6340, #3903, #1633, #5304, #6491, #4081, #1275, #3664, #641, #149 ),
 .UNSPECIFIED., .F., .F.,
 ( 4, 2, 2, 2, 2, 2, 2, 2, 4 ),
 ( 0.000000000000000000, 0.0002385177155853798715, 0.0004770354311707597429, 0.0009540708623415078849, 0.001431106293512256081, 0.001908141724683004277, 0.002385177155853752690, 0.002862212587024500886, 0.003816283449366009422 ),
 .UNSPECIFIED. ) ;
#3389 = AXIS2_PLACEMENT_3D ( 'NONE', #4170, #5277, #6390 ) ;
#3390 = CARTESIAN_POINT ( 'NONE',  ( 1.649606299212598381, 0.000000000000000000, 0.000000000000000000 ) ) ;
#3391 = CARTESIAN_POINT ( 'NONE',  ( 0.3531511627980793433, -0.1878266560944103492, 0.2783075040405565415 ) ) ;
#3392 = CARTESIAN_POINT ( 'NONE',  ( 0.9666437042230099363, 0.4330708661417423944, -1.454455828411337359 ) ) ;
#3393 = DIRECTION ( 'NONE',  ( -1.047444401652940007E-14, 1.000000000000000000, -4.625929269271482167E-15 ) ) ;
#3394 = ORIENTED_EDGE ( 'NONE', *, *, #6928, .F. ) ;
#3395 = CIRCLE ( 'NONE', #958, 0.4921259842519685179 ) ;
#3396 = CARTESIAN_POINT ( 'NONE',  ( 0.1171503679538647424, -0.3415090635818134879, -0.4046248963849241598 ) ) ;
#3397 = DIRECTION ( 'NONE',  ( 0.000000000000000000, 0.000000000000000000, -1.000000000000000000 ) ) ;
#3398 = CARTESIAN_POINT ( 'NONE',  ( 0.3565422129079688918, -0.1767726971815447856, -0.2952755905511810774 ) ) ;
#3399 = CARTESIAN_POINT ( 'NONE',  ( 0.000000000000000000, 0.2557161625347749712, -0.1476377952755909551 ) ) ;
#3400 = VECTOR ( 'NONE', #5647, 39.37007874015748143 ) ;
#3401 = CONTEXT_DEPENDENT_SHAPE_REPRESENTATION ( #2863, #3251 ) ;
#3402 = B_SPLINE_CURVE_WITH_KNOTS ( 'NONE', 3,
 ( #1044, #3960, #1103, #3919, #5145, #2729 ),
 .UNSPECIFIED., .F., .F.,
 ( 4, 2, 4 ),
 ( 0.000000000000000000, 0.0001677595217559110904, 0.0003355190435118221809 ),
 .UNSPECIFIED. ) ;
#3403 = EDGE_CURVE ( 'NONE', #2382, #1950, #6872, .T. ) ;
#3404 = CARTESIAN_POINT ( 'NONE',  ( 0.3432736861146661878, -0.3267484299055466446, -0.02460629921259840577 ) ) ;
#3405 = VERTEX_POINT ( 'NONE', #3848 ) ;
#3406 = DIRECTION ( 'NONE',  ( -0.000000000000000000, -1.000000000000000000, -0.000000000000000000 ) ) ;
#3407 = FACE_OUTER_BOUND ( 'NONE', #6659, .T. ) ;
#3408 = AXIS2_PLACEMENT_3D ( 'NONE', #2440, #1202, #3709 ) ;
#3409 = EDGE_LOOP ( 'NONE', ( #4393, #1468, #3865, #6476 ) ) ;
#3410 = ORIENTED_EDGE ( 'NONE', *, *, #3137, .T. ) ;
#3411 = CARTESIAN_POINT ( 'NONE',  ( 1.140380516255546706, -0.1779313096650642356, 0.9680979248264950376 ) ) ;
#3412 = VECTOR ( 'NONE', #190, 39.37007874015748143 ) ;
#3413 = EDGE_CURVE ( 'NONE', #813, #2163, #6469, .T. ) ;
#3414 = CARTESIAN_POINT ( 'NONE',  ( 0.3336175750056032396, 0.05682581389661631177, -0.2952755905511810219 ) ) ;
#3415 = ORIENTED_EDGE ( 'NONE', *, *, #1257, .F. ) ;
#3416 = EDGE_CURVE ( 'NONE', #5092, #2406, #1827, .T. ) ;
#3417 = DIRECTION ( 'NONE',  ( -2.207829878515936732E-15, 0.000000000000000000, 1.000000000000000000 ) ) ;
#3418 = ORIENTED_EDGE ( 'NONE', *, *, #711, .T. ) ;
#3419 = CARTESIAN_POINT ( 'NONE',  ( 1.218929327210600766, 0.03110856596261698734, 0.9838783093560928839 ) ) ;
#3420 = ADVANCED_FACE ( 'NONE', ( #2695 ), #2810, .T. ) ;
#3421 = ORIENTED_EDGE ( 'NONE', *, *, #6131, .F. ) ;
#3422 = CARTESIAN_POINT ( 'NONE',  ( 0.4685039370078740717, 0.3409548833797004797, 2.164902785881980513E-17 ) ) ;
#3423 = VERTEX_POINT ( 'NONE', #3238 ) ;
#3424 = DIRECTION ( 'NONE',  ( 0.000000000000000000, -0.000000000000000000, 1.000000000000000000 ) ) ;
#3425 = CARTESIAN_POINT ( 'NONE',  ( 25.35842062421581389, 45.20863634146751764, 54.79420970546445346 ) ) ;
#3426 = CARTESIAN_POINT ( 'NONE',  ( 0.000000000000000000, 1.496062992125984259, -0.7480314960629921295 ) ) ;
#3427 = EDGE_CURVE ( 'NONE', #448, #5027, #2681, .T. ) ;
#3428 = CARTESIAN_POINT ( 'NONE',  ( -0.1171503679538647702, 0.3415090635818126552, -0.4046248963849244373 ) ) ;
#3429 =( GEOMETRIC_REPRESENTATION_CONTEXT ( 3 ) GLOBAL_UNCERTAINTY_ASSIGNED_CONTEXT ( ( #1668 ) ) GLOBAL_UNIT_ASSIGNED_CONTEXT ( ( #5254, #3527, #5367 ) ) REPRESENTATION_CONTEXT ( 'NONE', 'WORKASPACE' ) );
#3430 = CARTESIAN_POINT ( 'NONE',  ( 0.000000000000000000, 0.000000000000000000, -0.4082677165354330340 ) ) ;
#3431 = CARTESIAN_POINT ( 'NONE',  ( 0.4509662133831519593, 0.9917530546321599028, -1.563429817131423594 ) ) ;
#3432 = FACE_BOUND ( 'NONE', #4461, .T. ) ;
#3433 = DIRECTION ( 'NONE',  ( 0.000000000000000000, 0.000000000000000000, -1.000000000000000000 ) ) ;
#3434 = AXIS2_PLACEMENT_3D ( 'NONE', #1781, #4122, #3673 ) ;
#3435 = FACE_OUTER_BOUND ( 'NONE', #5895, .T. ) ;
#3436 = CARTESIAN_POINT ( 'NONE',  ( -0.02890955082422800443, 0.3924549231051212561, -0.02201102547170738152 ) ) ;
#3437 = DIRECTION ( 'NONE',  ( -1.000000000000000000, -0.000000000000000000, -0.000000000000000000 ) ) ;
#3438 = AXIS2_PLACEMENT_3D ( 'NONE', #6648, #792, #4388 ) ;
#3439 = CONTEXT_DEPENDENT_SHAPE_REPRESENTATION ( #3540, #4288 ) ;
#3440 = CARTESIAN_POINT ( 'NONE',  ( -0.4406689276647596798, -0.9921522615226835429, -1.439080857166195271 ) ) ;
#3441 = VERTEX_POINT ( 'NONE', #2162 ) ;
#3442 = CARTESIAN_POINT ( 'NONE',  ( 0.000000000000000000, 1.496062992125984259, 0.000000000000000000 ) ) ;
#3443 = FACE_OUTER_BOUND ( 'NONE', #3291, .T. ) ;
#3444 = TOROIDAL_SURFACE ( 'NONE', #3830, 1.223643328182681289, 0.05905511811023622659 ) ;
#3445 = ORIENTED_EDGE ( 'NONE', *, *, #562, .F. ) ;
#3446 = AXIS2_PLACEMENT_3D ( 'NONE', #6960, #3516, #1101 ) ;
#3447 = EDGE_LOOP ( 'NONE', ( #5235, #2262 ) ) ;
#3448 = CARTESIAN_POINT ( 'NONE',  ( -3.198568410424924124, 2.407012729153881203, 2.480314960629921295 ) ) ;
#3449 = CIRCLE ( 'NONE', #4058, 1.278433327952054555 ) ;
#3450 = EDGE_LOOP ( 'NONE', ( #4203, #4244 ) ) ;
#3451 = FACE_OUTER_BOUND ( 'NONE', #3334, .T. ) ;
#3452 = DIRECTION ( 'NONE',  ( -1.000000000000000000, 0.000000000000000000, 0.000000000000000000 ) ) ;
#3453 = DIRECTION ( 'NONE',  ( -0.000000000000000000, -0.000000000000000000, 1.000000000000000000 ) ) ;
#3454 = ORIENTED_EDGE ( 'NONE', *, *, #2934, .F. ) ;
#3455 = AXIS2_PLACEMENT_3D ( 'NONE', #5554, #1366, #3747 ) ;
#3456 = EDGE_CURVE ( 'NONE', #6629, #7446, #6955, .T. ) ;
#3457 = ORIENTED_EDGE ( 'NONE', *, *, #6645, .T. ) ;
#3458 = DIRECTION ( 'NONE',  ( 0.000000000000000000, 1.000000000000000000, 0.000000000000000000 ) ) ;
#3459 = DIRECTION ( 'NONE',  ( -1.000000000000000000, -1.972152263052529514E-31, -4.151318482771456951E-16 ) ) ;
#3460 = CARTESIAN_POINT ( 'NONE',  ( 0.3505601438611543053, -0.3409548833797009237, 1.488710258487716964E-17 ) ) ;
#3461 = FACE_OUTER_BOUND ( 'NONE', #6741, .T. ) ;
#3462 = AXIS2_PLACEMENT_3D ( 'NONE', #7317, #5043, #3269 ) ;
#3463 = CARTESIAN_POINT ( 'NONE',  ( 0.3432736861146659102, 0.1846838951640040472, -0.2706692913385826404 ) ) ;
#3464 = ADVANCED_FACE ( 'NONE', ( #6948 ), #4145, .T. ) ;
#3465 = ADVANCED_FACE ( 'NONE', ( #7092 ), #4720, .T. ) ;
#3466 = AXIS2_PLACEMENT_3D ( 'NONE', #1150, #1121, #6908 ) ;
#3467 = EDGE_CURVE ( 'NONE', #811, #6826, #7318, .T. ) ;
#3468 = CARTESIAN_POINT ( 'NONE',  ( 0.3485777078273626373, -0.2029921329169081246, -0.2518088348849962799 ) ) ;
#3469 = DIRECTION ( 'NONE',  ( 0.000000000000000000, 0.000000000000000000, 1.000000000000000000 ) ) ;
#3470 = FACE_OUTER_BOUND ( 'NONE', #5419, .T. ) ;
#3471 = B_SPLINE_CURVE_WITH_KNOTS ( 'NONE', 3,
 ( #1634, #4476, #4045, #509, #6310, #6378, #3284, #385, #7101, #606 ),
 .UNSPECIFIED., .F., .F.,
 ( 4, 2, 2, 2, 4 ),
 ( 6.564673817405236669E-19, 0.002239656411828510989, 0.004479312823657021110, 0.006718969235485531231, 0.008958625647314040485 ),
 .UNSPECIFIED. ) ;
#3472 = AXIS2_PLACEMENT_3D ( 'NONE', #6986, #4195, #6449 ) ;
#3473 = CARTESIAN_POINT ( 'NONE',  ( -0.9479499796399322165, 0.4353079511162203374, -1.456692913385826849 ) ) ;
#3474 = CARTESIAN_POINT ( 'NONE',  ( 0.3336175750056032396, 0.2273032555864667459, 0.1968503937007873295 ) ) ;
#3475 = ITEM_DEFINED_TRANSFORMATION ( 'NONE', 'NONE', #5820,  #5166 ) ;
#3476 = LINE ( 'NONE', #5929, #2540 ) ;
#3477 = VERTEX_POINT ( 'NONE', #2469 ) ;
#3478 = CARTESIAN_POINT ( 'NONE',  ( -1.782879132931211256E-29, 1.702122929023921696E-15, -1.433776001880364026 ) ) ;
#3479 = DIRECTION ( 'NONE',  ( 0.000000000000000000, 0.000000000000000000, -1.000000000000000000 ) ) ;
#3480 = ORIENTED_EDGE ( 'NONE', *, *, #604, .T. ) ;
#3481 = EDGE_LOOP ( 'NONE', ( #5651, #5417, #1646, #6734 ) ) ;
#3482 = CARTESIAN_POINT ( 'NONE',  ( 1.060506290833840293, -0.2237082381425291866, 0.9584946220175588616 ) ) ;
#3483 = DIRECTION ( 'NONE',  ( 0.000000000000000000, 0.000000000000000000, -1.000000000000000000 ) ) ;
#3484 = ORIENTED_EDGE ( 'NONE', *, *, #2021, .T. ) ;
#3485 = CARTESIAN_POINT ( 'NONE',  ( -3.198568410424924124, 2.407012729153881203, 2.952755905511811108 ) ) ;
#3486 = CARTESIAN_POINT ( 'NONE',  ( 0.3485534891173986405, -0.1164145375797935450, 0.3017001449125945034 ) ) ;
#3487 = ORIENTED_EDGE ( 'NONE', *, *, #4071, .T. ) ;
#3488 = LINE ( 'NONE', #4000, #432 ) ;
#3489 = DIRECTION ( 'NONE',  ( -4.151318482771456951E-16, 1.972152263052529514E-31, 1.000000000000000000 ) ) ;
#3490 = PLANE ( 'NONE',  #1354 ) ;
#3491 = B_SPLINE_CURVE_WITH_KNOTS ( 'NONE', 3,
 ( #2512, #7172, #1942, #1361, #3707, #870, #5948, #2902, #5903, #6935 ),
 .UNSPECIFIED., .F., .F.,
 ( 4, 2, 2, 2, 4 ),
 ( 0.000000000000000000, 0.002239656411828510989, 0.004479312823657021977, 0.006718969235485534701, 0.008958625647314047424 ),
 .UNSPECIFIED. ) ;
#3492 = CARTESIAN_POINT ( 'NONE',  ( 0.01165389088405563781, -0.1143408654217081682, 0.2952755905511811885 ) ) ;
#3493 = CARTESIAN_POINT ( 'NONE',  ( 0.9055118110236223261, 0.7480314960629921295, 0.7480314960629921295 ) ) ;
#3494 = PRODUCT_RELATED_PRODUCT_CATEGORY ( 'part', '', ( #2384 ) ) ;
#3495 = PRODUCT_DEFINITION_FORMATION_WITH_SPECIFIED_SOURCE ( 'ANY', '', #2384, .NOT_KNOWN. ) ;
#3496 = DIRECTION ( 'NONE',  ( 2.207829878515936732E-15, -0.000000000000000000, -1.000000000000000000 ) ) ;
#3497 = ORIENTED_EDGE ( 'NONE', *, *, #2207, .F. ) ;
#3498 = DIRECTION ( 'NONE',  ( 0.000000000000000000, 0.000000000000000000, -1.000000000000000000 ) ) ;
#3499 = ADVANCED_FACE ( 'NONE', ( #1856 ), #1270, .F. ) ;
#3500 = DIRECTION ( 'NONE',  ( 1.000000000000000000, 0.000000000000000000, 0.000000000000000000 ) ) ;
#3501 = EDGE_CURVE ( 'NONE', #18, #322, #5748, .T. ) ;
#3502 = DIRECTION ( 'NONE',  ( -0.000000000000000000, -0.000000000000000000, 1.000000000000000000 ) ) ;
#3503 = EDGE_CURVE ( 'NONE', #781, #1792, #1699, .T. ) ;
#3504 = CARTESIAN_POINT ( 'NONE',  ( 3.027559055118110187, 2.428079244293728657E-17, -0.1982677165354330695 ) ) ;
#3505 = CARTESIAN_POINT ( 'NONE',  ( -0.4332839571663337774, 0.9726684123052331543, -1.452651065350217596 ) ) ;
#3506 = DIRECTION ( 'NONE',  ( 0.000000000000000000, 1.000000000000000000, 0.000000000000000000 ) ) ;
#3507 = CIRCLE ( 'NONE', #4724, 0.9842519685039370358 ) ;
#3508 = CARTESIAN_POINT ( 'NONE',  ( -0.4720886891211135139, -0.9960023578760586194, -1.401719942879701586 ) ) ;
#3509 = ADVANCED_FACE ( 'NONE', ( #5187, #2529 ), #4569, .T. ) ;
#3510 = ORIENTED_EDGE ( 'NONE', *, *, #744, .T. ) ;
#3511 = CARTESIAN_POINT ( 'NONE',  ( -0.4996352642496091345, -1.070877820178677498, -1.498503547059352403 ) ) ;
#3512 = FACE_BOUND ( 'NONE', #4559, .T. ) ;
#3513 = VERTEX_POINT ( 'NONE', #6107 ) ;
#3514 = CIRCLE ( 'NONE', #6939, 1.278433327952054555 ) ;
#3515 = ORIENTED_EDGE ( 'NONE', *, *, #7250, .F. ) ;
#3516 = DIRECTION ( 'NONE',  ( -0.000000000000000000, -0.000000000000000000, 1.000000000000000000 ) ) ;
#3517 = DIRECTION ( 'NONE',  ( -1.000000000000000000, -0.000000000000000000, -0.000000000000000000 ) ) ;
#3518 = ORIENTED_EDGE ( 'NONE', *, *, #4538, .F. ) ;
#3519 = VECTOR ( 'NONE', #4890, 39.37007874015748143 ) ;
#3520 = DIRECTION ( 'NONE',  ( 1.000000000000000000, 0.000000000000000000, -0.000000000000000000 ) ) ;
#3521 = PLANE ( 'NONE',  #6590 ) ;
#3522 = VERTEX_POINT ( 'NONE', #5503 ) ;
#3523 = PLANE ( 'NONE',  #5774 ) ;
#3524 = TOROIDAL_SURFACE ( 'NONE', #4018, 1.223643328182681289, 0.05905511811023622659 ) ;
#3525 = CARTESIAN_POINT ( 'NONE',  ( 0.3465690653189043013, 0.1180910924887165481, 0.2952755905511810774 ) ) ;
#3526 = APPLICATION_PROTOCOL_DEFINITION ( 'draft international standard', 'automotive_design', 1998, #1832 ) ;
#3527 =( NAMED_UNIT ( * ) PLANE_ANGLE_UNIT ( ) SI_UNIT ( $, .RADIAN. ) );
#3528 = DIRECTION ( 'NONE',  ( 1.000000000000000000, 0.000000000000000000, 0.000000000000000000 ) ) ;
#3529 = ORIENTED_EDGE ( 'NONE', *, *, #5272, .F. ) ;
#3530 = CARTESIAN_POINT ( 'NONE',  ( -0.4353079511162236681, -0.9479499796399322165, -1.456692913385828625 ) ) ;
#3531 = ORIENTED_EDGE ( 'NONE', *, *, #1486, .F. ) ;
#3532 = DIRECTION ( 'NONE',  ( 1.000000000000000000, 0.000000000000000000, 0.000000000000000000 ) ) ;
#3533 = VECTOR ( 'NONE', #5033, 39.37007874015748143 ) ;
#3534 = DIRECTION ( 'NONE',  ( 7.708596820178695308E-30, -2.207829878515936732E-15, 1.000000000000000000 ) ) ;
#3535 = CARTESIAN_POINT ( 'NONE',  ( 0.9411659768779468971, -0.4368170415251632077, -1.456692913385826849 ) ) ;
#3536 = AXIS2_PLACEMENT_3D ( 'NONE', #6904, #5192, #4534 ) ;
#3537 = DIRECTION ( 'NONE',  ( 0.000000000000000000, -0.000000000000000000, 1.000000000000000000 ) ) ;
#3538 = LINE ( 'NONE', #2310, #2718 ) ;
#3539 = CARTESIAN_POINT ( 'NONE',  ( 0.3510874053966554498, -0.1475872118127406207, -0.2952755905511810774 ) ) ;
#3540 =( REPRESENTATION_RELATIONSHIP ('NONE','NONE', #303, #7075 ) REPRESENTATION_RELATIONSHIP_WITH_TRANSFORMATION ( #5132 )SHAPE_REPRESENTATION_RELATIONSHIP( ) );
#3541 = CARTESIAN_POINT ( 'NONE',  ( -0.1469816153540869086, -0.3242859848650329058, -0.4082677165354330340 ) ) ;
#3542 = EDGE_CURVE ( 'NONE', #3331, #6705, #4466, .T. ) ;
#3543 = CARTESIAN_POINT ( 'NONE',  ( 0.4353079511162236126, -0.9479499796399308842, -1.456692913385826849 ) ) ;
#3544 = FACE_OUTER_BOUND ( 'NONE', #3603, .T. ) ;
#3545 = CIRCLE ( 'NONE', #2094, 1.089828288828796676 ) ;
#3546 = CARTESIAN_POINT ( 'NONE',  ( 0.3581828924050327045, -0.3486337532542230222, -1.123169198254405176E-18 ) ) ;
#3547 = CARTESIAN_POINT ( 'NONE',  ( 0.000000000000000000, 0.000000000000000000, -1.574803149606299302 ) ) ;
#3548 = DIRECTION ( 'NONE',  ( 0.000000000000000000, 8.881784197001249365E-16, 1.000000000000000000 ) ) ;
#3549 = ORIENTED_EDGE ( 'NONE', *, *, #5100, .T. ) ;
#3550 = PLANE ( 'NONE',  #6753 ) ;
#3551 = CARTESIAN_POINT ( 'NONE',  ( 6.500080172145040803E-30, -1.861696953619914682E-15, -1.361499588670820771 ) ) ;
#3552 = CONICAL_SURFACE ( 'NONE', #1105, 0.2952755905511810774, 1.047197551196600518 ) ;
#3553 = EDGE_CURVE ( 'NONE', #2829, #10, #6713, .T. ) ;
#3554 = EDGE_LOOP ( 'NONE', ( #3229, #5593, #5652, #6776, #7496, #3823 ) ) ;
#3555 = EDGE_CURVE ( 'NONE', #321, #6807, #2541, .T. ) ;
#3556 = DIRECTION ( 'NONE',  ( 0.000000000000000000, -0.000000000000000000, 1.000000000000000000 ) ) ;
#3557 = CARTESIAN_POINT ( 'NONE',  ( 0.000000000000000000, 0.2559055118110236116, 0.4921259842519685179 ) ) ;
#3558 = ORIENTED_EDGE ( 'NONE', *, *, #5479, .F. ) ;
#3559 = AXIS2_PLACEMENT_3D ( 'NONE', #4465, #940, #1620 ) ;
#3560 = CARTESIAN_POINT ( 'NONE',  ( 2.834645669291338876, 0.4724409448818890911, 2.480314960629921295 ) ) ;
#3561 = AXIS2_PLACEMENT_3D ( 'NONE', #4368, #4982, #7300 ) ;
#3562 = CARTESIAN_POINT ( 'NONE',  ( -0.5141614760841463072, -0.9609181420092334225, -1.361499588670821659 ) ) ;
#3563 = DIRECTION ( 'NONE',  ( 1.000000000000000000, 0.000000000000000000, -0.000000000000000000 ) ) ;
#3564 = ORIENTED_EDGE ( 'NONE', *, *, #6639, .T. ) ;
#3565 = CIRCLE ( 'NONE', #4177, 1.124634398195722973 ) ;
#3566 = FACE_OUTER_BOUND ( 'NONE', #4019, .T. ) ;
#3567 = CARTESIAN_POINT ( 'NONE',  ( 0.3398308759505395682, 0.1188917464549260616, 0.2952755905511810774 ) ) ;
#3568 = CARTESIAN_POINT ( 'NONE',  ( 0.3398308759505395682, 0.1188917464549260616, 0.2952755905511810774 ) ) ;
#3569 = ORIENTED_EDGE ( 'NONE', *, *, #6602, .T. ) ;
#3570 = CARTESIAN_POINT ( 'NONE',  ( -1.085749034322388118, -0.4630669964643945868, -1.535808346805854319 ) ) ;
#3571 = ORIENTED_EDGE ( 'NONE', *, *, #5109, .F. ) ;
#3572 = CIRCLE ( 'NONE', #7358, 0.9964144355006141485 ) ;
#3573 = FACE_OUTER_BOUND ( 'NONE', #7242, .T. ) ;
#3574 = ORIENTED_EDGE ( 'NONE', *, *, #4961, .F. ) ;
#3575 = ADVANCED_BREP_SHAPE_REPRESENTATION ( '', ( #1558, #5166 ), #3072 ) ;
#3576 = AXIS2_PLACEMENT_3D ( 'NONE', #1512, #3860, #6193 ) ;
#3577 = CARTESIAN_POINT ( 'NONE',  ( 0.000000000000000000, -0.2557161625347750822, -0.1476377952755907330 ) ) ;
#3578 = CARTESIAN_POINT ( 'NONE',  ( 1.048552902599916292, 0.4330708661417427274, -1.573978973432617279 ) ) ;
#3579 =( NAMED_UNIT ( * ) PLANE_ANGLE_UNIT ( ) SI_UNIT ( $, .RADIAN. ) );
#3580 = CARTESIAN_POINT ( 'NONE',  ( 0.000000000000000000, 0.000000000000000000, -1.546597720061111847 ) ) ;
#3581 = DIRECTION ( 'NONE',  ( -1.000000000000000000, 0.000000000000000000, 0.000000000000000000 ) ) ;
#3582 = CIRCLE ( 'NONE', #3097, 0.2952755905511810774 ) ;
#3583 = UNCERTAINTY_MEASURE_WITH_UNIT (LENGTH_MEASURE( 1.000000000000000082E-05 ), #4188, 'distance_accuracy_value', 'NONE');
#3584 = CARTESIAN_POINT ( 'NONE',  ( 2.834645669291338432, 0.000000000000000000, 0.000000000000000000 ) ) ;
#3585 = CARTESIAN_POINT ( 'NONE',  ( -0.4342019027940197673, 0.9783381746514265842, -1.450123259817210242 ) ) ;
#3586 = DIRECTION ( 'NONE',  ( 1.000000000000000000, 0.000000000000000000, 4.625929269271482167E-15 ) ) ;
#3587 = CARTESIAN_POINT ( 'NONE',  ( 0.4685039370078740717, -0.1704774416898499345, 0.2952755905511811330 ) ) ;
#3588 = CARTESIAN_POINT ( 'NONE',  ( 0.3410249605999788325, 0.02903799983316233957, 0.3014927230551917026 ) ) ;
#3589 = EDGE_LOOP ( 'NONE', ( #4979, #823, #5134, #1964 ) ) ;
#3590 = VECTOR ( 'NONE', #429, 39.37007874015748143 ) ;
#3591 = CARTESIAN_POINT ( 'NONE',  ( -0.4470329974975763010, -1.081428632361002951, -1.553789141944099894 ) ) ;
#3592 = ADVANCED_FACE ( 'NONE', ( #7246 ), #2432, .T. ) ;
#3593 = FACE_OUTER_BOUND ( 'NONE', #1617, .T. ) ;
#3594 = ORIENTED_EDGE ( 'NONE', *, *, #5809, .T. ) ;
#3595 = ORIENTED_EDGE ( 'NONE', *, *, #3315, .T. ) ;
#3596 = CIRCLE ( 'NONE', #2619, 0.4724409448818896462 ) ;
#3597 = CARTESIAN_POINT ( 'NONE',  ( 0.000000000000000000, 1.496062992125984259, -0.7480314960629921295 ) ) ;
#3598 = ORIENTED_EDGE ( 'NONE', *, *, #1576, .T. ) ;
#3599 = CARTESIAN_POINT ( 'NONE',  ( -0.3543307086614173040, -0.2045729300278205931, -0.03164754241312491001 ) ) ;
#3600 = EDGE_CURVE ( 'NONE', #3721, #3073, #6111, .T. ) ;
#3601 = ADVANCED_FACE ( 'NONE', ( #1422 ), #300, .T. ) ;
#3602 = ORIENTED_EDGE ( 'NONE', *, *, #6965, .T. ) ;
#3603 = EDGE_LOOP ( 'NONE', ( #1553, #3339 ) ) ;
#3604 = CARTESIAN_POINT ( 'NONE',  ( 0.9659644734970590507, -0.4700904924197804591, -1.546597720061111847 ) ) ;
#3605 = CARTESIAN_POINT ( 'NONE',  ( -0.2961551751698082713, 0.2381605899494506351, -0.3942397458900145368 ) ) ;
#3606 = ITEM_DEFINED_TRANSFORMATION ( 'NONE', 'NONE', #3559,  #5166 ) ;
#3607 = CARTESIAN_POINT ( 'NONE',  ( 0.3387173876318818611, 0.02883917696872971906, 0.2952755905511811330 ) ) ;
#3608 = CARTESIAN_POINT ( 'NONE',  ( -1.083410641227604554, -0.4508656291625843804, -1.549345754620972349 ) ) ;
#3609 = ORIENTED_EDGE ( 'NONE', *, *, #2479, .F. ) ;
#3610 = DIRECTION ( 'NONE',  ( -1.000000000000000000, 0.000000000000000000, 0.000000000000000000 ) ) ;
#3611 = PLANE ( 'NONE',  #1195 ) ;
#3612 = ORIENTED_EDGE ( 'NONE', *, *, #1081, .T. ) ;
#3613 =( NAMED_UNIT ( * ) PLANE_ANGLE_UNIT ( ) SI_UNIT ( $, .RADIAN. ) );
#3614 = PRODUCT ( 'Supporter', 'Supporter', '', ( #5366 ) ) ;
#3615 = CARTESIAN_POINT ( 'NONE',  ( 0.3337354549119980751, -0.2853048623713481113, -0.09638866382874244909 ) ) ;
#3616 = DIRECTION ( 'NONE',  ( 1.000000000000000000, 0.000000000000000000, 2.207829878515936732E-15 ) ) ;
#3617 = CARTESIAN_POINT ( 'NONE',  ( -1.075169953371344356, 0.4403524516313951920, -1.561970681382796045 ) ) ;
#3618 = FACE_OUTER_BOUND ( 'NONE', #4977, .T. ) ;
#3619 = CARTESIAN_POINT ( 'NONE',  ( 0.3391211773724056577, 0.1204696997606904962, -0.2952755905511810774 ) ) ;
#3620 = CARTESIAN_POINT ( 'NONE',  ( -0.4368378848980523088, -1.023372273685340117, -1.573834172653142183 ) ) ;
#3621 = CARTESIAN_POINT ( 'NONE',  ( 0.4437903857718327738, -0.9221073153504517617, -1.453484209829403850 ) ) ;
#3622 = DIRECTION ( 'NONE',  ( 1.000000000000000000, 0.000000000000000000, 0.000000000000000000 ) ) ;
#3623 = DIRECTION ( 'NONE',  ( -1.000000000000000000, -0.000000000000000000, 0.000000000000000000 ) ) ;
#3624 = FACE_OUTER_BOUND ( 'NONE', #1946, .T. ) ;
#3625 = CARTESIAN_POINT ( 'NONE',  ( 1.003669596044588941, -0.4445636273010707407, -1.568530023225017223 ) ) ;
#3626 = DIRECTION ( 'NONE',  ( 0.000000000000000000, 0.000000000000000000, -1.000000000000000000 ) ) ;
#3627 = CARTESIAN_POINT ( 'NONE',  ( 0.000000000000000000, 0.000000000000000000, 0.000000000000000000 ) ) ;
#3628 = ORIENTED_EDGE ( 'NONE', *, *, #5801, .T. ) ;
#3629 = CARTESIAN_POINT ( 'NONE',  ( 0.4330708661417322913, -0.9666437042230126009, -1.454455828411335583 ) ) ;
#3630 = DIRECTION ( 'NONE',  ( -1.000000000000000000, 0.000000000000000000, 0.000000000000000000 ) ) ;
#3631 = VERTEX_POINT ( 'NONE', #6641 ) ;
#3632 = CARTESIAN_POINT ( 'NONE',  ( -0.2066929133858267931, 2.531258147843938473E-17, 0.1188976377952756375 ) ) ;
#3633 = MECHANICAL_DESIGN_GEOMETRIC_PRESENTATION_REPRESENTATION (  '', ( #2404 ), #705 ) ;
#3634 = EDGE_CURVE ( 'NONE', #2767, #4636, #609, .T. ) ;
#3635 = DIRECTION ( 'NONE',  ( -1.000000000000000000, -0.000000000000000000, -0.000000000000000000 ) ) ;
#3636 = CARTESIAN_POINT ( 'NONE',  ( 1.968503937007874072, 0.000000000000000000, 0.000000000000000000 ) ) ;
#3637 = CYLINDRICAL_SURFACE ( 'NONE', #5129, 0.9842519685039370358 ) ;
#3638 = ORIENTED_EDGE ( 'NONE', *, *, #2764, .T. ) ;
#3639 = DIRECTION ( 'NONE',  ( 0.000000000000000000, 0.000000000000000000, -1.000000000000000000 ) ) ;
#3640 = ORIENTED_EDGE ( 'NONE', *, *, #6117, .T. ) ;
#3641 = ORIENTED_EDGE ( 'NONE', *, *, #793, .T. ) ;
#3642 = CARTESIAN_POINT ( 'NONE',  ( 0.3409812221349221573, -0.2754857644942658168, -0.1258275564122679768 ) ) ;
#3643 = CARTESIAN_POINT ( 'NONE',  ( 0.3565324925542818213, -0.1767206836160838956, 0.2952755905511811885 ) ) ;
#3644 = EDGE_CURVE ( 'NONE', #1383, #4734, #3675, .T. ) ;
#3645 = EDGE_CURVE ( 'NONE', #5971, #3323, #122, .T. ) ;
#3646 = APPLICATION_PROTOCOL_DEFINITION ( 'draft international standard', 'automotive_design', 1998, #3867 ) ;
#3647 = CARTESIAN_POINT ( 'NONE',  ( 2.755905511811024056, 0.000000000000000000, 0.7480314960629921295 ) ) ;
#3648 = EDGE_LOOP ( 'NONE', ( #293, #315, #2002 ) ) ;
#3649 = ADVANCED_FACE ( 'NONE', ( #5040 ), #944, .F. ) ;
#3650 = VERTEX_POINT ( 'NONE', #2054 ) ;
#3651 =( NAMED_UNIT ( * ) SI_UNIT ( $, .STERADIAN. ) SOLID_ANGLE_UNIT ( ) );
#3652 = APPLICATION_CONTEXT ( 'automotive_design' ) ;
#3653 = CIRCLE ( 'NONE', #361, 0.2362204724409448231 ) ;
#3654 = ORIENTED_EDGE ( 'NONE', *, *, #6171, .T. ) ;
#3655 = B_SPLINE_CURVE_WITH_KNOTS ( 'NONE', 3,
 ( #3599, #6, #1294, #659, #4092, #5248 ),
 .UNSPECIFIED., .F., .F.,
 ( 4, 2, 4 ),
 ( 0.009270618776430214827, 0.01189894710419331023, 0.01452727543195640389 ),
 .UNSPECIFIED. ) ;
#3656 = EDGE_CURVE ( 'NONE', #5946, #5590, #1331, .T. ) ;
#3657 = EDGE_CURVE ( 'NONE', #913, #1005, #2308, .T. ) ;
#3658 = DIRECTION ( 'NONE',  ( 0.000000000000000000, 0.000000000000000000, 1.000000000000000000 ) ) ;
#3659 = CARTESIAN_POINT ( 'NONE',  ( 0.3531511627980769008, -0.3349346966101605649, -0.02350890366535178522 ) ) ;
#3660 = CARTESIAN_POINT ( 'NONE',  ( 0.7723175066527832033, -0.1046133869837157365, -0.9787008116518934875 ) ) ;
#3661 = VECTOR ( 'NONE', #3702, 39.37007874015748143 ) ;
#3662 = CARTESIAN_POINT ( 'NONE',  ( 0.000000000000000000, 1.496062992125984259, 0.4921259842519685179 ) ) ;
#3663 = AXIS2_PLACEMENT_3D ( 'NONE', #2652, #412, #5077 ) ;
#3664 = CARTESIAN_POINT ( 'NONE',  ( 0.4999740374263536569, -0.9773781006402563198, -1.373989084483999257 ) ) ;
#3665 = DIRECTION ( 'NONE',  ( -2.207829878515936732E-15, 0.000000000000000000, 1.000000000000000000 ) ) ;
#3666 = CARTESIAN_POINT ( 'NONE',  ( 0.8785537298370166281, -0.4700904924197814028, -1.433776001880362250 ) ) ;
#3667 = DIRECTION ( 'NONE',  ( 1.000000000000000000, 0.000000000000000000, -0.000000000000000000 ) ) ;
#3668 = CARTESIAN_POINT ( 'NONE',  ( -0.2073036836782041203, -0.2894590224800286382, -0.0007480297793126502092 ) ) ;
#3669 = CARTESIAN_POINT ( 'NONE',  ( 0.3543307086614173596, -0.2045729300278204543, -0.3766201741223081378 ) ) ;
#3670 = CARTESIAN_POINT ( 'NONE',  ( 0.000000000000000000, 0.000000000000000000, 0.000000000000000000 ) ) ;
#3671 = ORIENTED_EDGE ( 'NONE', *, *, #1438, .F. ) ;
#3672 = DIRECTION ( 'NONE',  ( -1.047444401652940007E-14, 1.000000000000000000, -4.625929269271482167E-15 ) ) ;
#3673 = DIRECTION ( 'NONE',  ( 0.000000000000000000, 0.000000000000000000, 1.000000000000000000 ) ) ;
#3674 = EDGE_LOOP ( 'NONE', ( #2709, #6901, #1010, #546 ) ) ;
#3675 = B_SPLINE_CURVE_WITH_KNOTS ( 'NONE', 3,
 ( #2091, #3773, #1502, #5581, #1390, #2582, #4920, #4345 ),
 .UNSPECIFIED., .F., .F.,
 ( 4, 2, 2, 4 ),
 ( 0.004381617662950710798, 0.005472867551409541474, 0.006564117439868372150, 0.008746617216786031768 ),
 .UNSPECIFIED. ) ;
#3676 = B_SPLINE_CURVE_WITH_KNOTS ( 'NONE', 3,
 ( #6155, #5665, #1428, #2096, #264, #4966, #6759, #3779, #2660 ),
 .UNSPECIFIED., .F., .F.,
 ( 4, 2, 1, 2, 4 ),
 ( 2.312923578716022130E-20, 0.002165063509461098365, 0.004330127018922196730, 0.006495190528383295095, 0.008660254037844393460 ),
 .UNSPECIFIED. ) ;
#3677 = AXIS2_PLACEMENT_3D ( 'NONE', #2577, #3032, #743 ) ;
#3678 = LINE ( 'NONE', #3788, #753 ) ;
#3679 = CARTESIAN_POINT ( 'NONE',  ( 0.3581828924050323715, 0.1743168766271109560, 0.3019256869348722616 ) ) ;
#3680 = EDGE_LOOP ( 'NONE', ( #7311, #728 ) ) ;
#3681 = CARTESIAN_POINT ( 'NONE',  ( 0.4349192958999753555, 0.9810556462971140590, -1.448591228719267487 ) ) ;
#3682 = AXIS2_PLACEMENT_3D ( 'NONE', #1093, #2219, #2282 ) ;
#3683 = ORIENTED_EDGE ( 'NONE', *, *, #2255, .F. ) ;
#3684 = PRODUCT_DEFINITION_SHAPE ( 'NONE', 'NONE',  #7522 ) ;
#3685 = VERTEX_POINT ( 'NONE', #6073 ) ;
#3686 = DIRECTION ( 'NONE',  ( 0.000000000000000000, 1.000000000000000000, 0.000000000000000000 ) ) ;
#3687 = APPLICATION_PROTOCOL_DEFINITION ( 'draft international standard', 'automotive_design', 1998, #4437 ) ;
#3688 = AXIS2_PLACEMENT_3D ( 'NONE', #5386, #1819, #5811 ) ;
#3689 = DIRECTION ( 'NONE',  ( -0.000000000000000000, -0.000000000000000000, 1.000000000000000000 ) ) ;
#3690 = CARTESIAN_POINT ( 'NONE',  ( 3.027559055118110187, 0.000000000000000000, 0.000000000000000000 ) ) ;
#3691 = AXIS2_PLACEMENT_3D ( 'NONE', #4660, #6927, #1166 ) ;
#3692 = VERTEX_POINT ( 'NONE', #3309 ) ;
#3693 = DIRECTION ( 'NONE',  ( -1.000000000000000000, -0.000000000000000000, -0.000000000000000000 ) ) ;
#3694 = EDGE_CURVE ( 'NONE', #7275, #4992, #220, .T. ) ;
#3695 = PRESENTATION_LAYER_ASSIGNMENT (  '', '', ( #7343 ) ) ;
#3696 = AXIS2_PLACEMENT_3D ( 'NONE', #140, #4803, #4532 ) ;
#3697 = ORIENTED_EDGE ( 'NONE', *, *, #7432, .T. ) ;
#3698 = CARTESIAN_POINT ( 'NONE',  ( 0.3543307086614172485, 0.000000000000000000, 7.886165872636028972E-17 ) ) ;
#3699 = SURFACE_STYLE_FILL_AREA ( #4267 ) ;
#3700 = CIRCLE ( 'NONE', #7468, 1.168853328413307358 ) ;
#3701 = CARTESIAN_POINT ( 'NONE',  ( 0.4330708661417322913, -1.048552902599920289, -1.573978973432616835 ) ) ;
#3702 = DIRECTION ( 'NONE',  ( -1.000000000000000000, -0.000000000000000000, -0.000000000000000000 ) ) ;
#3703 = EDGE_CURVE ( 'NONE', #5110, #5853, #6842, .T. ) ;
#3704 = EDGE_CURVE ( 'NONE', #2899, #1531, #4883, .T. ) ;
#3705 = DIRECTION ( 'NONE',  ( 0.000000000000000000, 1.000000000000000000, 0.000000000000000000 ) ) ;
#3706 = CARTESIAN_POINT ( 'NONE',  ( 0.3581828924050323715, 0.1743168766271109560, 0.3019256869348722616 ) ) ;
#3707 = CARTESIAN_POINT ( 'NONE',  ( 0.3410076799406683845, 0.2467857494855107137, -0.1755389823809322958 ) ) ;
#3708 = CARTESIAN_POINT ( 'NONE',  ( 1.968503937007874072, 1.496062992125984259, 0.000000000000000000 ) ) ;
#3709 = DIRECTION ( 'NONE',  ( -1.000000000000000000, 0.000000000000000000, 0.000000000000000000 ) ) ;
#3710 = LINE ( 'NONE', #799, #3519 ) ;
#3711 = ORIENTED_EDGE ( 'NONE', *, *, #187, .F. ) ;
#3712 = PLANE ( 'NONE',  #4800 ) ;
#3713 = DIRECTION ( 'NONE',  ( -1.000000000000000000, -0.000000000000000000, -0.000000000000000000 ) ) ;
#3714 =( BOUNDED_SURFACE ( )  B_SPLINE_SURFACE ( 3, 2, ( 
 ( #5867, #3066, #592 ),
 ( #2341, #4752, #628 ),
 ( #4832, #178, #2909 ),
 ( #7159, #3607, #4138 ),
 ( #6475, #1929, #7125 ),
 ( #3568, #668, #7084 ),
 ( #704, #1845, #6522 ),
 ( #5255, #4260, #6596 ) ),
 .UNSPECIFIED., .F., .F., .F. ) 
 B_SPLINE_SURFACE_WITH_KNOTS ( ( 4, 2, 2, 4 ),
 ( 3, 3 ),
 ( 0.03551233549299846748, 0.03994185813602711688, 0.04215661945754144158, 0.04437138077905577321 ),
 ( 0.000000000000000000, 1.000000000000000000 ),
 .UNSPECIFIED. ) 
 GEOMETRIC_REPRESENTATION_ITEM ( )  RATIONAL_B_SPLINE_SURFACE ( (
 ( 1.000000000000000000, 0.8047781229087798138, 1.000000000000000000),
 ( 1.000000000000000000, 0.8123782171506571670, 1.000000000000000000),
 ( 1.000000000000000000, 0.8190665209243362943, 1.000000000000000000),
 ( 1.000000000000000000, 0.8191935049886309717, 1.000000000000000000),
 ( 1.000000000000000000, 0.8176088963536531917, 1.000000000000000000),
 ( 1.000000000000000000, 0.8122958360081882212, 1.000000000000000000),
 ( 1.000000000000000000, 0.8086309270602213273, 1.000000000000000000),
 ( 1.000000000000000000, 0.8047712437947333042, 1.000000000000000000) ) ) 
 REPRESENTATION_ITEM ( '' )  SURFACE ( )  );
#3715 = EDGE_LOOP ( 'NONE', ( #3598, #4973, #4909, #5750, #247, #3571 ) ) ;
#3716 = LINE ( 'NONE', #1995, #45 ) ;
#3717 = CARTESIAN_POINT ( 'NONE',  ( 0.3398315730591770500, -0.1188962366173021562, -0.2952755905511810774 ) ) ;
#3718 = CARTESIAN_POINT ( 'NONE',  ( 0.7480314960629921295, -0.007724973897226917324, 0.9842519685039369248 ) ) ;
#3719 = AXIS2_PLACEMENT_3D ( 'NONE', #880, #6660, #3862 ) ;
#3720 = CARTESIAN_POINT ( 'NONE',  ( 3.027559055118110187, 0.000000000000000000, 0.000000000000000000 ) ) ;
#3721 = VERTEX_POINT ( 'NONE', #7314 ) ;
#3722 = CARTESIAN_POINT ( 'NONE',  ( 0.3387177083556421331, 0.2412911239081777792, -0.1726226950780199998 ) ) ;
#3723 = EDGE_LOOP ( 'NONE', ( #6128, #3976, #3954, #3257 ) ) ;
#3724 = CIRCLE ( 'NONE', #2016, 0.2362204724409448231 ) ;
#3725 = ORIENTED_EDGE ( 'NONE', *, *, #5490, .F. ) ;
#3726 = CARTESIAN_POINT ( 'NONE',  ( 0.3388536909603144798, -0.2250264928541644005, -0.2007938624299156205 ) ) ;
#3727 =( LENGTH_UNIT ( ) NAMED_UNIT ( * ) SI_UNIT ( $, .METRE. ) );
#3728 = ORIENTED_EDGE ( 'NONE', *, *, #6273, .F. ) ;
#3729 = CARTESIAN_POINT ( 'NONE',  ( 0.3459463601587901560, 0.1956820507697113742, 0.2516199270399913090 ) ) ;
#3730 = ORIENTED_EDGE ( 'NONE', *, *, #1078, .F. ) ;
#3731 = CARTESIAN_POINT ( 'NONE',  ( 21.65354330708661479, 6.026805113914139867E-17, -0.4921259842519685179 ) ) ;
#3732 = DIRECTION ( 'NONE',  ( -0.000000000000000000, -0.000000000000000000, 1.000000000000000000 ) ) ;
#3733 = EDGE_LOOP ( 'NONE', ( #4521, #4088, #5358, #472 ) ) ;
#3734 = ADVANCED_FACE ( 'NONE', ( #4599 ), #5078, .F. ) ;
#3735 = DIRECTION ( 'NONE',  ( 0.000000000000000000, 0.000000000000000000, -1.000000000000000000 ) ) ;
#3736 = DIRECTION ( 'NONE',  ( -1.000000000000000000, 0.000000000000000000, 0.000000000000000000 ) ) ;
#3737 = B_SPLINE_CURVE_WITH_KNOTS ( 'NONE', 3,
 ( #5453, #5568, #4292, #2607, #1339, #2644 ),
 .UNSPECIFIED., .F., .F.,
 ( 4, 2, 4 ),
 ( -3.269571951034336179E-06, 0.0001651384380483830793, 0.0003335464480478004612 ),
 .UNSPECIFIED. ) ;
#3738 = FACE_OUTER_BOUND ( 'NONE', #5646, .T. ) ;
#3739 = EDGE_CURVE ( 'NONE', #7262, #6925, #3040, .T. ) ;
#3740 = ADVANCED_FACE ( 'NONE', ( #7467 ), #2204, .T. ) ;
#3741 = CARTESIAN_POINT ( 'NONE',  ( 0.4526810454163319730, 0.9044351468059360633, -1.447629383090422772 ) ) ;
#3742 = LINE ( 'NONE', #3587, #5136 ) ;
#3743 = CARTESIAN_POINT ( 'NONE',  ( -0.2962704110120348289, -0.2380940585049214631, -0.01405589313879346096 ) ) ;
#3744 = DIRECTION ( 'NONE',  ( 0.000000000000000000, 0.000000000000000000, -1.000000000000000000 ) ) ;
#3745 = DIRECTION ( 'NONE',  ( 0.000000000000000000, 0.000000000000000000, 1.000000000000000000 ) ) ;
#3746 = ORIENTED_EDGE ( 'NONE', *, *, #4026, .T. ) ;
#3747 = DIRECTION ( 'NONE',  ( 0.000000000000000000, 0.000000000000000000, 1.000000000000000000 ) ) ;
#3748 = EDGE_CURVE ( 'NONE', #4293, #6087, #4395, .T. ) ;
#3749 = CARTESIAN_POINT ( 'NONE',  ( -0.4508657589754699324, 1.083410700381146174, -1.549345605342071774 ) ) ;
#3750 = PRODUCT_DEFINITION_FORMATION_WITH_SPECIFIED_SOURCE ( 'ANY', '', #5591, .NOT_KNOWN. ) ;
#3751 = EDGE_LOOP ( 'NONE', ( #124, #5097, #3911, #6468 ) ) ;
#3752 = CARTESIAN_POINT ( 'NONE',  ( 0.02637295201093707228, -0.1704774416898499345, 0.2952755905511811330 ) ) ;
#3753 = CARTESIAN_POINT ( 'NONE',  ( 0.4685039370078740717, 0.000000000000000000, 0.4507874015748032370 ) ) ;
#3754 = EDGE_CURVE ( 'NONE', #4474, #2045, #1954, .T. ) ;
#3755 = DIRECTION ( 'NONE',  ( 0.000000000000000000, 0.000000000000000000, 1.000000000000000000 ) ) ;
#3756 = VERTEX_POINT ( 'NONE', #6399 ) ;
#3757 = CARTESIAN_POINT ( 'NONE',  ( 0.3465694189146783510, 0.1966695024996976682, -0.2499096104736449331 ) ) ;
#3758 = B_SPLINE_CURVE_WITH_KNOTS ( 'NONE', 3,
 ( #4056, #2263, #5788, #5140, #6282, #4021, #5243, #549, #7453, #2, #1071, #3411, #1134, #2229, #5208, #5751, #3482, #6994, #2933, #7157, #1041, #3373, #4598, #6895, #4089, #5275, #38, #2363, #1648, #4698, #1610, #3955, #517, #3992, #5180, #7490, #1288, #5896, #1372, #1330, #693, #5315, #3718, #1209 ),
 .UNSPECIFIED., .F., .F.,
 ( 4, 2, 2, 2, 2, 2, 2, 2, 2, 2, 2, 2, 2, 2, 2, 2, 2, 2, 2, 2, 2, 4 ),
 ( 4.896973959386981381E-19, 0.001176728898091255592, 0.001765093347136882304, 0.002353457796182509016, 0.003530186694273764608, 0.004706915592365020634, 0.005883644490456278395, 0.007060373388547535288, 0.007648737837593169372, 0.008237102286638802590, 0.009413831184730070759, 0.01059056008282133893, 0.01176728898091260710, 0.01235565342995824031, 0.01294401787900387527, 0.01353238232804950848, 0.01412074677709514170, 0.01529747567518641160, 0.01647420457327768151, 0.01765093347136895141, 0.01823929792041458289, 0.01882766236946021784 ),
 .UNSPECIFIED. ) ;
#3759 = ORIENTED_EDGE ( 'NONE', *, *, #5150, .F. ) ;
#3760 = PRESENTATION_LAYER_ASSIGNMENT (  '', '', ( #1785 ) ) ;
#3761 = VERTEX_POINT ( 'NONE', #2737 ) ;
#3762 = CARTESIAN_POINT ( 'NONE',  ( 0.3543307086614173040, 0.2045729300278205931, -0.3766201741223081378 ) ) ;
#3763 = CARTESIAN_POINT ( 'NONE',  ( 0.2073490933073314779, -0.2894328052184282352, -3.494844601269712023E-17 ) ) ;
#3764 = CARTESIAN_POINT ( 'NONE',  ( 0.9971724964170014527, -0.4476001829032997259, -1.429776958199368453 ) ) ;
#3765 = VERTEX_POINT ( 'NONE', #5700 ) ;
#3766 = CIRCLE ( 'NONE', #98, 1.278433327952055887 ) ;
#3767 = CARTESIAN_POINT ( 'NONE',  ( 0.3483227611829848303, 0.3409548833797004797, 0.000000000000000000 ) ) ;
#3768 = ORIENTED_EDGE ( 'NONE', *, *, #2715, .T. ) ;
#3769 = CARTESIAN_POINT ( 'NONE',  ( 0.3485373078438442351, -0.2031105961982146157, 0.2516016230262508313 ) ) ;
#3770 = ORIENTED_EDGE ( 'NONE', *, *, #3034, .F. ) ;
#3771 = AXIS2_PLACEMENT_3D ( 'NONE', #4886, #1984, #2966 ) ;
#3772 = SHAPE_REPRESENTATION_RELATIONSHIP ( 'NONE' , 'NONE' ,  #5265, #5868 ) ;
#3773 = CARTESIAN_POINT ( 'NONE',  ( -2.403706095987794643E-16, 0.2484822268960368286, -0.1601673393405684265 ) ) ;
#3774 = ADVANCED_BREP_SHAPE_REPRESENTATION ( '', ( #1517, #5166 ), #879 ) ;
#3775 = VECTOR ( 'NONE', #2460, 39.37007874015748143 ) ;
#3776 = DIRECTION ( 'NONE',  ( 0.000000000000000000, 0.000000000000000000, -1.000000000000000000 ) ) ;
#3777 = DIRECTION ( 'NONE',  ( -1.000000000000000000, -0.000000000000000000, 0.000000000000000000 ) ) ;
#3778 = AXIS2_PLACEMENT_3D ( 'NONE', #6968, #5283, #552 ) ;
#3779 = CARTESIAN_POINT ( 'NONE',  ( 0.3432736861146659102, 0.1846838951640040472, -0.2706692913385826404 ) ) ;
#3780 = CARTESIAN_POINT ( 'NONE',  ( 0.3425764178929368575, 0.2900721174007582781, 0.1006592143205869566 ) ) ;
#3781 = CARTESIAN_POINT ( 'NONE',  ( 0.9659644734970493918, 0.4700904924198003876, -1.546597720061112069 ) ) ;
#3782 = ORIENTED_EDGE ( 'NONE', *, *, #7229, .F. ) ;
#3783 = DIRECTION ( 'NONE',  ( 1.000000000000000000, 0.000000000000000000, 4.625929269271482167E-15 ) ) ;
#3784 = CARTESIAN_POINT ( 'NONE',  ( 0.3483227611829848303, 0.3409548833797004797, 0.000000000000000000 ) ) ;
#3785 = ADVANCED_FACE ( 'NONE', ( #1659, #531 ), #1114, .F. ) ;
#3786 = ORIENTED_EDGE ( 'NONE', *, *, #3941, .T. ) ;
#3787 = DIRECTION ( 'NONE',  ( -0.000000000000000000, -1.000000000000000000, 0.000000000000000000 ) ) ;
#3788 = CARTESIAN_POINT ( 'NONE',  ( 0.3997746709170348356, 0.000000000000000000, -0.4629062255509093782 ) ) ;
#3789 = TOROIDAL_SURFACE ( 'NONE', #5752, 1.223643328182682621, 0.05905511811023622659 ) ;
#3790 = CARTESIAN_POINT ( 'NONE',  ( 1.649606299212598381, 0.000000000000000000, 0.000000000000000000 ) ) ;
#3791 = ORIENTED_EDGE ( 'NONE', *, *, #1537, .T. ) ;
#3792 = CARTESIAN_POINT ( 'NONE',  ( 0.3483227611829849413, -0.3409548833797009237, 0.000000000000000000 ) ) ;
#3793 = EDGE_CURVE ( 'NONE', #6892, #4433, #4369, .T. ) ;
#3794 = EDGE_CURVE ( 'NONE', #2762, #6349, #1015, .T. ) ;
#3795 = EDGE_LOOP ( 'NONE', ( #848, #2182, #5241, #7366 ) ) ;
#3796 = VERTEX_POINT ( 'NONE', #1143 ) ;
#3797 = CARTESIAN_POINT ( 'NONE',  ( 0.01171324505787554697, -0.1984117137466534231, 0.2468920120763462012 ) ) ;
#3798 = ORIENTED_EDGE ( 'NONE', *, *, #2521, .T. ) ;
#3799 = CARTESIAN_POINT ( 'NONE',  ( -0.3543307086614173040, 0.000000000000000000, 7.886165872636028972E-17 ) ) ;
#3800 = EDGE_LOOP ( 'NONE', ( #6478, #3415, #6168, #114, #6291 ) ) ;
#3801 = AXIS2_PLACEMENT_3D ( 'NONE', #2359, #1327, #5889 ) ;
#3802 = CARTESIAN_POINT ( 'NONE',  ( -0.3543307086614173040, -0.03456946083495022332, -0.4082677165354330895 ) ) ;
#3803 = ORIENTED_EDGE ( 'NONE', *, *, #5197, .F. ) ;
#3804 = DIRECTION ( 'NONE',  ( 0.000000000000000000, 0.000000000000000000, 1.000000000000000000 ) ) ;
#3805 = ORIENTED_EDGE ( 'NONE', *, *, #2480, .T. ) ;
#3806 = ORIENTED_EDGE ( 'NONE', *, *, #187, .T. ) ;
#3807 = AXIS2_PLACEMENT_3D ( 'NONE', #6078, #5430, #3201 ) ;
#3808 = PRODUCT_DEFINITION_SHAPE ( 'NONE', 'NONE',  #7531 ) ;
#3809 = DIRECTION ( 'NONE',  ( 0.000000000000000000, 0.000000000000000000, 1.000000000000000000 ) ) ;
#3810 = DIRECTION ( 'NONE',  ( -0.000000000000000000, -0.000000000000000000, 1.000000000000000000 ) ) ;
#3811 = AXIS2_PLACEMENT_3D ( 'NONE', #5921, #5839, #566 ) ;
#3812 = CIRCLE ( 'NONE', #4905, 0.2831409772408586822 ) ;
#3813 = DIRECTION ( 'NONE',  ( 0.000000000000000000, 0.000000000000000000, -1.000000000000000000 ) ) ;
#3814 = VECTOR ( 'NONE', #4571, 39.37007874015748143 ) ;
#3815 = UNCERTAINTY_MEASURE_WITH_UNIT (LENGTH_MEASURE( 1.000000000000000082E-05 ), #1664, 'distance_accuracy_value', 'NONE');
#3816 = CARTESIAN_POINT ( 'NONE',  ( 3.027559055118110187, 0.000000000000000000, 0.1982677165354330695 ) ) ;
#3817 = VECTOR ( 'NONE', #2495, 39.37007874015748143 ) ;
#3818 = CARTESIAN_POINT ( 'NONE',  ( 0.8833138556571487054, -0.4663806185498647894, -1.436938405272744079 ) ) ;
#3819 = CARTESIAN_POINT ( 'NONE',  ( 1.279527559055118280, 1.968503937007874072, 0.4724409448818898127 ) ) ;
#3820 = FACE_OUTER_BOUND ( 'NONE', #2398, .T. ) ;
#3821 = CARTESIAN_POINT ( 'NONE',  ( 1.968503937007874072, 0.000000000000000000, 0.2362204724409449619 ) ) ;
#3822 = CARTESIAN_POINT ( 'NONE',  ( -0.4349482935633079972, 1.030265555772311048, -1.574803149606299302 ) ) ;
#3823 = ORIENTED_EDGE ( 'NONE', *, *, #2330, .T. ) ;
#3824 = CARTESIAN_POINT ( 'NONE',  ( 0.3336175750056034617, -0.2841290694830839736, 0.09842519685039370636 ) ) ;
#3825 = CIRCLE ( 'NONE', #415, 1.174991162294038771 ) ;
#3826 = ORIENTED_EDGE ( 'NONE', *, *, #2711, .F. ) ;
#3827 = CARTESIAN_POINT ( 'NONE',  ( -0.1171503679538647841, 0.3415090635818126552, -0.003642820150508618762 ) ) ;
#3828 = CARTESIAN_POINT ( 'NONE',  ( 0.002479217192763490639, -0.05744896992510376693, -0.2952755905511810774 ) ) ;
#3829 = ITEM_DEFINED_TRANSFORMATION ( 'NONE', 'NONE', #7219,  #5166 ) ;
#3830 = AXIS2_PLACEMENT_3D ( 'NONE', #5624, #2169, #5702 ) ;
#3831 = PRODUCT_DEFINITION ( 'UNKNOWN', '', #6075, #680 ) ;
#3832 = CARTESIAN_POINT ( 'NONE',  ( 0.4403525121893732686, 1.075170037517933164, -1.561970602951607168 ) ) ;
#3833 = ORIENTED_EDGE ( 'NONE', *, *, #4541, .F. ) ;
#3834 = DIRECTION ( 'NONE',  ( 0.000000000000000000, 0.000000000000000000, 1.000000000000000000 ) ) ;
#3835 = ORIENTED_EDGE ( 'NONE', *, *, #2530, .T. ) ;
#3836 = ORIENTED_EDGE ( 'NONE', *, *, #4211, .T. ) ;
#3837 = CONICAL_SURFACE ( 'NONE', #5794, 0.4629062255509093782, 1.221730476396037490 ) ;
#3838 = CARTESIAN_POINT ( 'NONE',  ( 0.01171324505787584534, -0.3130206113228972131, -0.04838357847483532731 ) ) ;
#3839 = CARTESIAN_POINT ( 'NONE',  ( 0.000000000000000000, 0.000000000000000000, 0.000000000000000000 ) ) ;
#3840 = ADVANCED_FACE ( 'NONE', ( #4501 ), #4030, .T. ) ;
#3841 = ADVANCED_FACE ( 'NONE', ( #5658 ), #6296, .F. ) ;
#3842 = CARTESIAN_POINT ( 'NONE',  ( 0.9983959133492292803, -0.4514965799695651039, -1.424958590981960205 ) ) ;
#3843 = VERTEX_POINT ( 'NONE', #5156 ) ;
#3844 = CARTESIAN_POINT ( 'NONE',  ( 0.7480314960629922405, 0.01544581072159242723, 0.9842519685039369248 ) ) ;
#3845 = CIRCLE ( 'NONE', #5917, 0.2362204724409449341 ) ;
#3846 = ORIENTED_EDGE ( 'NONE', *, *, #4497, .F. ) ;
#3847 = DIRECTION ( 'NONE',  ( 0.9991895563372418243, -0.04025208698423509562, 8.530088470570894506E-16 ) ) ;
#3848 = CARTESIAN_POINT ( 'NONE',  ( 0.9609181420092280934, 0.5141614760841562992, -1.361499588670821659 ) ) ;
#3849 = CARTESIAN_POINT ( 'NONE',  ( 3.198568410424924124, 2.407012729153881203, 2.952755905511811108 ) ) ;
#3850 = CARTESIAN_POINT ( 'NONE',  ( 0.8656462225360395113, -0.2048623079342055120, -0.9627353284137957212 ) ) ;
#3851 = CARTESIAN_POINT ( 'NONE',  ( 0.4330708661417322913, 1.048552902599920289, -1.573978973432616835 ) ) ;
#3852 = CARTESIAN_POINT ( 'NONE',  ( 0.7965081100895167188, 0.1441822837186601813, -0.9737193899100770045 ) ) ;
#3853 = B_SPLINE_CURVE_WITH_KNOTS ( 'NONE', 3,
 ( #2702, #5550, #834, #7400, #5047, #3163 ),
 .UNSPECIFIED., .F., .F.,
 ( 4, 2, 4 ),
 ( 2.380732026380333730E-07, 0.002190927868076681349, 0.004381617662950723809 ),
 .UNSPECIFIED. ) ;
#3854 = CARTESIAN_POINT ( 'NONE',  ( 0.1771653543307088463, 0.3068593950417300431, 7.886165872636028972E-17 ) ) ;
#3855 = CARTESIAN_POINT ( 'NONE',  ( 0.000000000000000000, 0.000000000000000000, 0.000000000000000000 ) ) ;
#3856 = CARTESIAN_POINT ( 'NONE',  ( 0.3398312250857989381, -0.1962691648279019652, 0.2506030156613254789 ) ) ;
#3857 = CARTESIAN_POINT ( 'NONE',  ( 0.4685039370078740717, 0.000000000000000000, 0.2362204724409449064 ) ) ;
#3858 = CARTESIAN_POINT ( 'NONE',  ( 1.003668447264486563, 0.4445641707283079502, -1.568529612473645418 ) ) ;
#3859 = ORIENTED_EDGE ( 'NONE', *, *, #5162, .T. ) ;
#3860 = DIRECTION ( 'NONE',  ( -0.000000000000000000, -0.000000000000000000, 1.000000000000000000 ) ) ;
#3861 = EDGE_LOOP ( 'NONE', ( #402, #5537, #3093, #1499 ) ) ;
#3862 = DIRECTION ( 'NONE',  ( 0.000000000000000000, 0.000000000000000000, 1.000000000000000000 ) ) ;
#3863 = DIRECTION ( 'NONE',  ( 1.000000000000000000, 0.000000000000000000, -0.000000000000000000 ) ) ;
#3864 = CARTESIAN_POINT ( 'NONE',  ( -0.9971723906835420204, -0.4475999628372231975, -1.429777239771659270 ) ) ;
#3865 = ORIENTED_EDGE ( 'NONE', *, *, #4450, .F. ) ;
#3866 = DIRECTION ( 'NONE',  ( 0.000000000000000000, 0.000000000000000000, 1.000000000000000000 ) ) ;
#3867 = APPLICATION_CONTEXT ( 'automotive_design' ) ;
#3868 = DIRECTION ( 'NONE',  ( 0.000000000000000000, -0.000000000000000000, -1.000000000000000000 ) ) ;
#3869 = ORIENTED_EDGE ( 'NONE', *, *, #5844, .F. ) ;
#3870 = ORIENTED_EDGE ( 'NONE', *, *, #1246, .F. ) ;
#3871 =( CONVERSION_BASED_UNIT ( 'INCH', #2264 ) LENGTH_UNIT ( ) NAMED_UNIT ( #2183 ) );
#3872 = EDGE_LOOP ( 'NONE', ( #1456, #1095, #2410 ) ) ;
#3873 = CARTESIAN_POINT ( 'NONE',  ( 0.4330708661417322913, 0.9666437042230126009, -1.454455828411335583 ) ) ;
#3874 = ORIENTED_EDGE ( 'NONE', *, *, #6131, .T. ) ;
#3875 = CARTESIAN_POINT ( 'NONE',  ( 0.8656462225360395113, 0.2048623079342055120, 0.9627353284137957212 ) ) ;
#3876 = ORIENTED_EDGE ( 'NONE', *, *, #4496, .F. ) ;
#3877 = CARTESIAN_POINT ( 'NONE',  ( 0.3387177083556158763, 0.2701412011613934516, 0.1226528954731279514 ) ) ;
#3878 = CARTESIAN_POINT ( 'NONE',  ( 7.874015748031496287, 0.000000000000000000, 0.2362204724409455170 ) ) ;
#3879 = VERTEX_POINT ( 'NONE', #6330 ) ;
#3880 = EDGE_CURVE ( 'NONE', #4570, #7420, #276, .T. ) ;
#3881 = ORIENTED_EDGE ( 'NONE', *, *, #4716, .F. ) ;
#3882 = EDGE_CURVE ( 'NONE', #3362, #2406, #7319, .T. ) ;
#3883 = LINE ( 'NONE', #7354, #1506 ) ;
#3884 = DIRECTION ( 'NONE',  ( 1.000000000000000000, 0.000000000000000000, 0.000000000000000000 ) ) ;
#3885 = AXIS2_PLACEMENT_3D ( 'NONE', #6354, #3295, #518 ) ;
#3886 = CARTESIAN_POINT ( 'NONE',  ( 0.2948818897637794922, 0.000000000000000000, 0.1783464566929134354 ) ) ;
#3887 = EDGE_CURVE ( 'NONE', #1388, #7025, #556, .T. ) ;
#3888 = DIRECTION ( 'NONE',  ( 1.000000000000000000, 0.000000000000000000, 0.000000000000000000 ) ) ;
#3889 = CARTESIAN_POINT ( 'NONE',  ( 1.220472440944882164, -0.01566504975835071242, -0.9842519685039374799 ) ) ;
#3890 = DIRECTION ( 'NONE',  ( -1.000000000000000000, 0.000000000000000000, 0.000000000000000000 ) ) ;
#3891 = AXIS2_PLACEMENT_3D ( 'NONE', #1602, #6276, #2789 ) ;
#3892 = ADVANCED_FACE ( 'NONE', ( #5909 ), #130, .F. ) ;
#3893 = EDGE_CURVE ( 'NONE', #34, #614, #5482, .T. ) ;
#3894 = CARTESIAN_POINT ( 'NONE',  ( 0.4349482935633082747, 1.030265555772310826, -1.574803149606299302 ) ) ;
#3895 = CARTESIAN_POINT ( 'NONE',  ( 0.3483227611829846082, 0.1704774416898497680, -0.2952755905511810774 ) ) ;
#3896 = AXIS2_PLACEMENT_3D ( 'NONE', #3627, #5472, #4321 ) ;
#3897 = DIRECTION ( 'NONE',  ( 0.000000000000000000, 0.000000000000000000, -1.000000000000000000 ) ) ;
#3898 = LINE ( 'NONE', #1629, #830 ) ;
#3899 = ORIENTED_EDGE ( 'NONE', *, *, #891, .T. ) ;
#3900 = CARTESIAN_POINT ( 'NONE',  ( 0.01836325778988323956, -0.1427310470019406141, 0.2952755905511810774 ) ) ;
#3901 = VERTEX_POINT ( 'NONE', #2457 ) ;
#3902 = AXIS2_PLACEMENT_3D ( 'NONE', #2551, #7024, #1778 ) ;
#3903 = CARTESIAN_POINT ( 'NONE',  ( 0.4596433552321258498, -0.9990286922241453649, -1.415369843883346412 ) ) ;
#3904 = DIRECTION ( 'NONE',  ( -1.000000000000000000, -0.000000000000000000, -0.000000000000000000 ) ) ;
#3905 = ITEM_DEFINED_TRANSFORMATION ( 'NONE', 'NONE', #4657,  #5166 ) ;
#3906 = CARTESIAN_POINT ( 'NONE',  ( -0.9983958463931797978, -0.4514963146295112306, -1.424958914991361736 ) ) ;
#3907 = EDGE_LOOP ( 'NONE', ( #3803, #3989, #6084, #2442 ) ) ;
#3908 = CARTESIAN_POINT ( 'NONE',  ( 0.3411151615605715337, 0.2917056203871458142, -0.09774174715358552312 ) ) ;
#3909 = AXIS2_PLACEMENT_3D ( 'NONE', #4690, #7060, #2921 ) ;
#3910 = DIRECTION ( 'NONE',  ( 1.000000000000000000, 0.000000000000000000, 0.000000000000000000 ) ) ;
#3911 = ORIENTED_EDGE ( 'NONE', *, *, #4071, .F. ) ;
#3912 = ORIENTED_EDGE ( 'NONE', *, *, #4674, .F. ) ;
#3913 = MANIFOLD_SOLID_BREP ( 'FlangeHexFillet', #3968 ) ;
#3914 = DIRECTION ( 'NONE',  ( 1.000000000000000000, 0.000000000000000000, 0.000000000000000000 ) ) ;
#3915 = AXIS2_PLACEMENT_3D ( 'NONE', #5731, #6975, #4574 ) ;
#3916 = CARTESIAN_POINT ( 'NONE',  ( 0.9983959133492219529, 0.4514965799695863091, -1.424958590981962425 ) ) ;
#3917 = FACE_OUTER_BOUND ( 'NONE', #2126, .T. ) ;
#3918 = ORIENTED_EDGE ( 'NONE', *, *, #4860, .F. ) ;
#3919 = CARTESIAN_POINT ( 'NONE',  ( 0.3561392902752972267, 0.1723302545757742221, 0.2984847566065203517 ) ) ;
#3920 = ORIENTED_EDGE ( 'NONE', *, *, #2655, .F. ) ;
#3921 = CARTESIAN_POINT ( 'NONE',  ( -0.1771653543307089018, -0.3068593950417300986, -0.4082677165354330340 ) ) ;
#3922 = ORIENTED_EDGE ( 'NONE', *, *, #3370, .F. ) ;
#3923 = CARTESIAN_POINT ( 'NONE',  ( 0.3479980290963966549, 0.2016732288369792181, 0.2541005850305664282 ) ) ;
#3924 = ORIENTED_EDGE ( 'NONE', *, *, #5161, .T. ) ;
#3925 = CARTESIAN_POINT ( 'NONE',  ( 33.78363125245377319, 38.11143353299877390, 52.63397348499202621 ) ) ;
#3926 = AXIS2_PLACEMENT_3D ( 'NONE', #5515, #313, #6086 ) ;
#3927 = DIRECTION ( 'NONE',  ( 0.000000000000000000, 1.000000000000000000, 0.000000000000000000 ) ) ;
#3928 = MANIFOLD_SOLID_BREP ( 'Boss-Extrude2', #4682 ) ;
#3929 = PRESENTATION_STYLE_ASSIGNMENT (( #5732 ) ) ;
#3930 = ADVANCED_FACE ( 'NONE', ( #5988 ), #3789, .T. ) ;
#3931 = CARTESIAN_POINT ( 'NONE',  ( 3.198568410424924124, 2.407012729153881203, 0.4724409448818898127 ) ) ;
#3932 =( LENGTH_UNIT ( ) NAMED_UNIT ( * ) SI_UNIT ( $, .METRE. ) );
#3933 = CARTESIAN_POINT ( 'NONE',  ( 0.4685039370078740717, -0.1704774416898505729, -0.2952755905511810774 ) ) ;
#3934 = AXIS2_PLACEMENT_3D ( 'NONE', #1318, #3777, #868 ) ;
#3935 = EDGE_CURVE ( 'NONE', #1079, #1691, #1720, .T. ) ;
#3936 = FACE_OUTER_BOUND ( 'NONE', #1923, .T. ) ;
#3937 = CARTESIAN_POINT ( 'NONE',  ( -0.4627504720074766542, -0.8884022185686314410, -1.439912370850675138 ) ) ;
#3938 = EDGE_CURVE ( 'NONE', #3721, #34, #1255, .T. ) ;
#3939 = VECTOR ( 'NONE', #5451, 39.37007874015748143 ) ;
#3940 = DIRECTION ( 'NONE',  ( 0.000000000000000000, 1.000000000000000000, 0.000000000000000000 ) ) ;
#3941 = EDGE_CURVE ( 'NONE', #2077, #1762, #1930, .T. ) ;
#3942 = EDGE_LOOP ( 'NONE', ( #1080, #3259, #5068, #6627, #1656, #6013, #7493, #6481, #6381, #971, #7145, #2118 ) ) ;
#3943 = AXIS2_PLACEMENT_3D ( 'NONE', #6964, #4061, #1046 ) ;
#3944 = CARTESIAN_POINT ( 'NONE',  ( -0.8989373009621118849, 0.4559215864680308816, -1.445239633971734383 ) ) ;
#3945 = DIRECTION ( 'NONE',  ( -1.000000000000000000, -0.000000000000000000, -0.000000000000000000 ) ) ;
#3946 = DIRECTION ( 'NONE',  ( 0.000000000000000000, -4.440892098500625373E-15, 1.000000000000000000 ) ) ;
#3947 = ORIENTED_EDGE ( 'NONE', *, *, #1494, .F. ) ;
#3948 = AXIS2_PLACEMENT_3D ( 'NONE', #726, #5888, #6384 ) ;
#3950 = CARTESIAN_POINT ( 'NONE',  ( 0.3585665126877354281, 0.1732820025503171713, -0.3037348580927971553 ) ) ;
#3949 = DIMENSIONAL_EXPONENTS ( 1.000000000000000000, 0.000000000000000000, 0.000000000000000000, 0.000000000000000000, 0.000000000000000000, 0.000000000000000000, 0.000000000000000000 ) ;
#3951 = CARTESIAN_POINT ( 'NONE',  ( 0.3510872220067887683, 0.1819230426404221390, -0.2754512281816320352 ) ) ;
#3952 = APPLICATION_CONTEXT ( 'automotive_design' ) ;
#3953 = ORIENTED_EDGE ( 'NONE', *, *, #2021, .F. ) ;
#3954 = ORIENTED_EDGE ( 'NONE', *, *, #5065, .T. ) ;
#3955 = CARTESIAN_POINT ( 'NONE',  ( 0.8284312913633176123, -0.1777059077220142780, 0.9680895064399986927 ) ) ;
#3956 = CARTESIAN_POINT ( 'NONE',  ( 0.3581828924050323715, 0.1743168766271109560, 0.3019256869348722616 ) ) ;
#3957 = B_SPLINE_CURVE_WITH_KNOTS ( 'NONE', 3,
 ( #3080, #7167, #374, #5080, #1662, #2656 ),
 .UNSPECIFIED., .F., .F.,
 ( 4, 2, 4 ),
 ( 2.380730968228221197E-07, 0.002629065763328360898, 0.005257893453559898435 ),
 .UNSPECIFIED. ) ;
#3958 = FACE_OUTER_BOUND ( 'NONE', #5606, .T. ) ;
#3959 = EDGE_LOOP ( 'NONE', ( #1410, #4371, #3480, #5822 ) ) ;
#3960 = CARTESIAN_POINT ( 'NONE',  ( 0.3505602286436571013, 0.1704774416898499345, 0.2952755905511810774 ) ) ;
#3961 = ORIENTED_EDGE ( 'NONE', *, *, #4067, .F. ) ;
#3962 = CARTESIAN_POINT ( 'NONE',  ( 1.162034203329631143, 0.1562967039942805003, 0.9718251695195749829 ) ) ;
#3963 = ORIENTED_EDGE ( 'NONE', *, *, #7428, .T. ) ;
#3964 =( BOUNDED_SURFACE ( )  B_SPLINE_SURFACE ( 3, 2, ( 
 ( #1298, #3643, #2372 ),
 ( #5986, #738, #2907 ),
 ( #4136, #4097, #588 ),
 ( #12, #7004, #1842 ),
 ( #85, #1176, #1263 ),
 ( #3567, #3525, #2413 ),
 ( #1218, #5864, #4706 ),
 ( #7039, #1794, #4749 ) ),
 .UNSPECIFIED., .F., .F., .F. ) 
 B_SPLINE_SURFACE_WITH_KNOTS ( ( 4, 2, 2, 4 ),
 ( 3, 3 ),
 ( 0.03551233549299846748, 0.03994185813602711688, 0.04215661945754144158, 0.04437138077905577321 ),
 ( 0.000000000000000000, 1.000000000000000000 ),
 .UNSPECIFIED. ) 
 GEOMETRIC_REPRESENTATION_ITEM ( )  RATIONAL_B_SPLINE_SURFACE ( (
 ( 1.000000000000000000, 0.8047781229087798138, 1.000000000000000000),
 ( 1.000000000000000000, 0.8123782171506571670, 1.000000000000000000),
 ( 1.000000000000000000, 0.8190665209243362943, 1.000000000000000000),
 ( 1.000000000000000000, 0.8191935049886309717, 1.000000000000000000),
 ( 1.000000000000000000, 0.8176088963536531917, 1.000000000000000000),
 ( 1.000000000000000000, 0.8122958360081882212, 1.000000000000000000),
 ( 1.000000000000000000, 0.8086309270602213273, 1.000000000000000000),
 ( 1.000000000000000000, 0.8047712437947333042, 1.000000000000000000) ) ) 
 REPRESENTATION_ITEM ( '' )  SURFACE ( )  );
#3965 = CARTESIAN_POINT ( 'NONE',  ( 0.3485616995351332181, -0.1165012447190267864, -0.3017003685801735724 ) ) ;
#3966 = CARTESIAN_POINT ( 'NONE',  ( 27.32692456123183433, 45.20863634146260068, 52.37806797318098972 ) ) ;
#3967 = CARTESIAN_POINT ( 'NONE',  ( 0.8989373009621074440, 0.4559215864680435937, -1.445239633971736604 ) ) ;
#3968 = CLOSED_SHELL ( 'NONE', ( #2373, #2430, #4307, #694, #3509, #3465, #1587, #4353, #4962, #3740, #6454, #7134, #1300, #3592, #1962, #6179, #4595, #1355, #4635, #533, #5440, #4955, #5724, #2331, #752, #1714, #6092, #6646, #5564 ) ) ;
#3969 = CARTESIAN_POINT ( 'NONE',  ( 0.0006233585804809438748, -0.2412158484082067011, 0.1727530760685163091 ) ) ;
#3970 = CARTESIAN_POINT ( 'NONE',  ( 0.8794895096619267383, 0.2118599820681134061, -0.9611874069187010816 ) ) ;
#3971 = CIRCLE ( 'NONE', #4687, 0.2066929133858267931 ) ;
#3972 =( NAMED_UNIT ( * ) PLANE_ANGLE_UNIT ( ) SI_UNIT ( $, .RADIAN. ) );
#3973 = CARTESIAN_POINT ( 'NONE',  ( -0.3543307086614173040, 0.2045729300278199547, -0.03164754241312472960 ) ) ;
#3974 = CARTESIAN_POINT ( 'NONE',  ( 0.3322361761492158561, -0.2866471735583170366, 0.09406371265334383114 ) ) ;
#3975 = PLANE ( 'NONE',  #5344 ) ;
#3976 = ORIENTED_EDGE ( 'NONE', *, *, #1754, .T. ) ;
#3977 = LINE ( 'NONE', #1057, #4922 ) ;
#3978 = EDGE_CURVE ( 'NONE', #4277, #6588, #3105, .T. ) ;
#3979 = ORIENTED_EDGE ( 'NONE', *, *, #4716, .T. ) ;
#3980 = DIRECTION ( 'NONE',  ( 7.708596820178695308E-30, -2.207829878515936732E-15, 1.000000000000000000 ) ) ;
#3981 = EDGE_CURVE ( 'NONE', #2932, #5946, #2006, .T. ) ;
#3982 = EDGE_CURVE ( 'NONE', #4654, #3879, #2633, .T. ) ;
#3983 = CARTESIAN_POINT ( 'NONE',  ( 1.968503937007874072, 0.000000000000000000, 0.000000000000000000 ) ) ;
#3984 = EDGE_CURVE ( 'NONE', #1603, #4456, #1450, .T. ) ;
#3985 = CARTESIAN_POINT ( 'NONE',  ( -0.4330708661417321803, -0.9697097640641213490, -1.453662949853145481 ) ) ;
#3986 = ORIENTED_EDGE ( 'NONE', *, *, #6306, .T. ) ;
#3987 = CARTESIAN_POINT ( 'NONE',  ( 0.01832242175888466190, -0.1844213691142429778, -0.2711239997950803393 ) ) ;
#3988 = CARTESIAN_POINT ( 'NONE',  ( 0.3487102105009278197, -0.2024297391849458061, 0.2527898980517221394 ) ) ;
#3989 = ORIENTED_EDGE ( 'NONE', *, *, #6117, .F. ) ;
#3990 = ORIENTED_EDGE ( 'NONE', *, *, #95, .T. ) ;
#3991 = EDGE_CURVE ( 'NONE', #4166, #7153, #2651, .T. ) ;
#3992 = CARTESIAN_POINT ( 'NONE',  ( 0.8062392625377295952, -0.1560493051692869171, 0.9718662726019896558 ) ) ;
#3993 =( NAMED_UNIT ( * ) PLANE_ANGLE_UNIT ( ) SI_UNIT ( $, .RADIAN. ) );
#3994 = ORIENTED_EDGE ( 'NONE', *, *, #1596, .T. ) ;
#3995 = DIRECTION ( 'NONE',  ( 1.000000000000000000, 0.000000000000000000, -0.000000000000000000 ) ) ;
#3996 = ORIENTED_EDGE ( 'NONE', *, *, #565, .F. ) ;
#3997 = CARTESIAN_POINT ( 'NONE',  ( -0.1771653543307089573, 0.3068593950417301541, 0.000000000000000000 ) ) ;
#3998 = ORIENTED_EDGE ( 'NONE', *, *, #5476, .T. ) ;
#3999 = VERTEX_POINT ( 'NONE', #6670 ) ;
#4000 = CARTESIAN_POINT ( 'NONE',  ( 2.755905511811024056, 1.496062992125984259, -0.2362204724409449896 ) ) ;
#4001 = DIRECTION ( 'NONE',  ( 0.000000000000000000, 0.000000000000000000, -1.000000000000000000 ) ) ;
#4002 = CARTESIAN_POINT ( 'NONE',  ( 0.9479499796399277756, 0.4353079511162336046, -1.456692913385828625 ) ) ;
#4003 = CARTESIAN_POINT ( 'NONE',  ( 0.4921259842519683514, 0.000000000000000000, -2.204724409448820754 ) ) ;
#4004 = FILL_AREA_STYLE_COLOUR ( '', #2336 ) ;
#4005 = CARTESIAN_POINT ( 'NONE',  ( -0.3543307086614173040, 0.1714946277491095350, -0.02209865905065006367 ) ) ;
#4006 = DIRECTION ( 'NONE',  ( 0.000000000000000000, 1.000000000000000000, 0.000000000000000000 ) ) ;
#4007 = AXIS2_PLACEMENT_3D ( 'NONE', #1362, #6575, #4238 ) ;
#4008 = CARTESIAN_POINT ( 'NONE',  ( 0.000000000000000000, 2.957312202238506242E-17, 0.2952755905511810774 ) ) ;
#4009 = CARTESIAN_POINT ( 'NONE',  ( 0.4475999628372195893, -0.9971723906835419093, -1.429777239771657271 ) ) ;
#4010 = CARTESIAN_POINT ( 'NONE',  ( 0.3485534891173986405, -0.1164145375797935450, 0.3017001449125945034 ) ) ;
#4011 = CIRCLE ( 'NONE', #7303, 1.278433327952056553 ) ;
#4012 = VECTOR ( 'NONE', #532, 39.37007874015748143 ) ;
#4013 = CARTESIAN_POINT ( 'NONE',  ( -0.4349192646538860285, -0.9810555383103382043, -1.448591292758283133 ) ) ;
#4014 = ORIENTED_EDGE ( 'NONE', *, *, #496, .F. ) ;
#4015 = FACE_OUTER_BOUND ( 'NONE', #6516, .T. ) ;
#4016 = CARTESIAN_POINT ( 'NONE',  ( 0.3585569128062321420, -0.3496569568119795024, -0.001755940978325754281 ) ) ;
#4017 = EDGE_CURVE ( 'NONE', #1108, #4739, #1061, .T. ) ;
#4018 = AXIS2_PLACEMENT_3D ( 'NONE', #6576, #1467, #6191 ) ;
#4019 = EDGE_LOOP ( 'NONE', ( #3730, #5376, #5021, #7346 ) ) ;
#4020 = VERTEX_POINT ( 'NONE', #324 ) ;
#4021 = CARTESIAN_POINT ( 'NONE',  ( 1.207998888640173130, -0.07614347099379424610, 0.9813305615101511892 ) ) ;
#4022 = CIRCLE ( 'NONE', #975, 0.3543307086614173596 ) ;
#4023 = CARTESIAN_POINT ( 'NONE',  ( 0.003035684155427062578, 0.2268414356900468054, -0.1976502892253328703 ) ) ;
#4024 = ORIENTED_EDGE ( 'NONE', *, *, #1863, .T. ) ;
#4025 = CARTESIAN_POINT ( 'NONE',  ( 0.4685039370078740717, 2.892866454678787531E-17, -0.2362204724409449064 ) ) ;
#4026 = EDGE_CURVE ( 'NONE', #6209, #5498, #3737, .T. ) ;
#4027 = EDGE_CURVE ( 'NONE', #5096, #7070, #817, .T. ) ;
#4028 = CARTESIAN_POINT ( 'NONE',  ( 9.857707340795016185E-18, -0.4091458600556410752, -0.4082677165354330340 ) ) ;
#4029 = ORIENTED_EDGE ( 'NONE', *, *, #496, .T. ) ;
#4030 = TOROIDAL_SURFACE ( 'NONE', #730, 1.043121362164705745, 0.05905511811023622659 ) ;
#4031 = CARTESIAN_POINT ( 'NONE',  ( 0.000000000000000000, 0.000000000000000000, 0.000000000000000000 ) ) ;
#4032 = CARTESIAN_POINT ( 'NONE',  ( 0.000000000000000000, 0.000000000000000000, 0.1783464566929134354 ) ) ;
#4033 = MANIFOLD_SOLID_BREP ( 'Fillet2', #2613 ) ;
#4034 = SURFACE_SIDE_STYLE ('',( #4502 ) ) ;
#4035 = COLOUR_RGB ( '',0.7921568627450980005, 0.8196078431372548767, 0.9333333333333333481 ) ;
#4036 = CARTESIAN_POINT ( 'NONE',  ( 0.5118110236220474452, 1.220472440944881942, 2.480314960629921295 ) ) ;
#4037 = CARTESIAN_POINT ( 'NONE',  ( -1.010074371201531429, -0.4416272204091005738, -1.570717485485532583 ) ) ;
#4038 = B_SPLINE_CURVE_WITH_KNOTS ( 'NONE', 3,
 ( #7495, #2268, #5792, #3486, #5249, #5695 ),
 .UNSPECIFIED., .F., .F.,
 ( 4, 2, 4 ),
 ( 0.004466737480205772853, 0.006712681563759903200, 0.008958625647314033547 ),
 .UNSPECIFIED. ) ;
#4039 = APPLICATION_CONTEXT ( 'automotive_design' ) ;
#4040 = CARTESIAN_POINT ( 'NONE',  ( 0.3410076799406688286, -0.2754140928391124454, -0.1259532371559686781 ) ) ;
#4041 = DIRECTION ( 'NONE',  ( 1.000000000000000000, 0.000000000000000000, 0.000000000000000000 ) ) ;
#4042 = AXIS2_PLACEMENT_3D ( 'NONE', #4263, #2462, #1894 ) ;
#4043 = CARTESIAN_POINT ( 'NONE',  ( 0.3409815385080205985, -0.02878389060673587282, -0.3014914578570770387 ) ) ;
#4044 = CARTESIAN_POINT ( 'NONE',  ( -0.9221077491748242982, 0.4437902010346525539, -1.453484313640521552 ) ) ;
#4045 = CARTESIAN_POINT ( 'NONE',  ( 0.3485373078438445127, -0.3194486952732369378, -0.05009812457233156491 ) ) ;
#4046 = AXIS2_PLACEMENT_3D ( 'NONE', #5054, #2748, #5090 ) ;
#4047 = AXIS2_PLACEMENT_3D ( 'NONE', #6016, #6624, #2111 ) ;
#4048 = CARTESIAN_POINT ( 'NONE',  ( -0.5141614760841463072, -0.9609181420092334225, -1.361499588670821659 ) ) ;
#4049 = EDGE_LOOP ( 'NONE', ( #2566, #4354, #4525 ) ) ;
#4050 = LINE ( 'NONE', #1708, #2906 ) ;
#4051 = LINE ( 'NONE', #7113, #1861 ) ;
#4052 = CONICAL_SURFACE ( 'NONE', #4301, 0.2952755905511810774, 1.047197551196600518 ) ;
#4053 = CARTESIAN_POINT ( 'NONE',  ( 0.000000000000000000, 0.000000000000000000, -1.515748031496062964 ) ) ;
#4054 = VERTEX_POINT ( 'NONE', #2232 ) ;
#4055 = EDGE_LOOP ( 'NONE', ( #3172, #4717, #1452, #2008, #4946, #3230, #3638 ) ) ;
#4056 = CARTESIAN_POINT ( 'NONE',  ( 1.220472440944881720, -1.984939871850715226E-17, 0.9842519685039370358 ) ) ;
#4057 = PRODUCT_RELATED_PRODUCT_CATEGORY ( 'part', '', ( #2452 ) ) ;
#4058 = AXIS2_PLACEMENT_3D ( 'NONE', #365, #2686, #4952 ) ;
#4059 = CARTESIAN_POINT ( 'NONE',  ( -0.3543307086614173040, -0.2045729300278205931, -0.3766201741223081378 ) ) ;
#4060 = ORIENTED_EDGE ( 'NONE', *, *, #481, .F. ) ;
#4061 = DIRECTION ( 'NONE',  ( -1.000000000000000000, -0.000000000000000000, -4.625929269271482167E-15 ) ) ;
#4062 = FACE_OUTER_BOUND ( 'NONE', #3213, .T. ) ;
#4063 = EDGE_LOOP ( 'NONE', ( #5151, #5936, #7425, #2913 ) ) ;
#4064 = CIRCLE ( 'NONE', #5546, 0.7480314960629921295 ) ;
#4065 = DIRECTION ( 'NONE',  ( 0.000000000000000000, 0.8660254037844375974, -0.5000000000000018874 ) ) ;
#4066 = ADVANCED_FACE ( 'NONE', ( #3958 ), #7267, .F. ) ;
#4067 = EDGE_CURVE ( 'NONE', #3843, #1950, #5014, .T. ) ;
#4068 = DIRECTION ( 'NONE',  ( 1.000000000000000000, 0.000000000000000000, 0.000000000000000000 ) ) ;
#4069 = DIRECTION ( 'NONE',  ( -1.000000000000000000, -0.000000000000000000, -0.000000000000000000 ) ) ;
#4070 = CARTESIAN_POINT ( 'NONE',  ( -0.1771653543307089573, 0.3068593950417301541, -0.4082677165354330340 ) ) ;
#4071 = EDGE_CURVE ( 'NONE', #4636, #2767, #825, .T. ) ;
#4072 = CARTESIAN_POINT ( 'NONE',  ( -1.702122929023921696E-15, 0.000000000000000000, -1.433776001880364026 ) ) ;
#4073 = EDGE_CURVE ( 'NONE', #2290, #5576, #953, .T. ) ;
#4074 =( LENGTH_UNIT ( ) NAMED_UNIT ( * ) SI_UNIT ( $, .METRE. ) );
#4075 = CIRCLE ( 'NONE', #782, 0.03543307086614165546 ) ;
#4076 = CARTESIAN_POINT ( 'NONE',  ( 0.000000000000000000, 0.2557161625347749712, -0.1476377952755909551 ) ) ;
#4077 = CARTESIAN_POINT ( 'NONE',  ( 0.3997746709170348356, 0.000000000000000000, 0.000000000000000000 ) ) ;
#4078 = DIRECTION ( 'NONE',  ( -0.000000000000000000, -0.000000000000000000, 1.000000000000000000 ) ) ;
#4079 = CARTESIAN_POINT ( 'NONE',  ( 0.000000000000000000, 0.2559055118110236116, 0.000000000000000000 ) ) ;
#4080 = MANIFOLD_SOLID_BREP ( 'Cut-Extrude1', #2971 ) ;
#4081 = CARTESIAN_POINT ( 'NONE',  ( 0.4843356560173194270, -0.9895441027518980803, -1.389133886014302099 ) ) ;
#4082 = DIRECTION ( 'NONE',  ( 0.000000000000000000, 0.000000000000000000, 1.000000000000000000 ) ) ;
#4083 = CARTESIAN_POINT ( 'NONE',  ( 0.000000000000000000, 0.000000000000000000, 0.000000000000000000 ) ) ;
#4084 = ORIENTED_EDGE ( 'NONE', *, *, #4027, .F. ) ;
#4085 = CARTESIAN_POINT ( 'NONE',  ( -0.4878045971889968246, -1.078368813366570755, -1.510181706589752260 ) ) ;
#4086 = CARTESIAN_POINT ( 'NONE',  ( 2.755905511811024056, 1.496062992125984259, 0.2362204724409449896 ) ) ;
#4087 = ORIENTED_EDGE ( 'NONE', *, *, #1247, .T. ) ;
#4088 = ORIENTED_EDGE ( 'NONE', *, *, #2848, .F. ) ;
#4089 = CARTESIAN_POINT ( 'NONE',  ( 0.9080621969490132450, -0.2241341580870719608, 0.9584117186519856002 ) ) ;
#4090 = DIRECTION ( 'NONE',  ( -1.000000000000000000, 0.000000000000000000, 0.000000000000000000 ) ) ;
#4091 = ORIENTED_EDGE ( 'NONE', *, *, #2522, .T. ) ;
#4092 = CARTESIAN_POINT ( 'NONE',  ( -0.3543307086614173040, -0.03456946083495023719, 4.441920810010739880E-17 ) ) ;
#4093 = CARTESIAN_POINT ( 'NONE',  ( -0.4700904924197903401, -0.9659644734970543878, -1.546597720061111847 ) ) ;
#4094 = CARTESIAN_POINT ( 'NONE',  ( 0.9842519685039370358, 1.220472440944881942, 0.000000000000000000 ) ) ;
#4095 = ORIENTED_EDGE ( 'NONE', *, *, #3739, .T. ) ;
#4096 = DIRECTION ( 'NONE',  ( 0.000000000000000000, 0.000000000000000000, 1.000000000000000000 ) ) ;
#4097 = CARTESIAN_POINT ( 'NONE',  ( 0.3388543739203577765, -0.06138491293039709945, 0.2952755905511811330 ) ) ;
#4098 =( NAMED_UNIT ( * ) PLANE_ANGLE_UNIT ( ) SI_UNIT ( $, .RADIAN. ) );
#4099 = DIRECTION ( 'NONE',  ( -4.625929269271482167E-15, 0.000000000000000000, 1.000000000000000000 ) ) ;
#4100 = DIRECTION ( 'NONE',  ( 0.000000000000000000, 0.000000000000000000, 1.000000000000000000 ) ) ;
#4101 = ORIENTED_EDGE ( 'NONE', *, *, #2617, .F. ) ;
#4102 = CARTESIAN_POINT ( 'NONE',  ( 1.085572762089316079, -0.4589126309195263320, -1.540322683979783003 ) ) ;
#4103 = EDGE_LOOP ( 'NONE', ( #5994, #7033, #3168, #6204 ) ) ;
#4104 = DIRECTION ( 'NONE',  ( 1.000000000000000000, 0.000000000000000000, 0.000000000000000000 ) ) ;
#4105 = EDGE_CURVE ( 'NONE', #5789, #725, #5375, .T. ) ;
#4106 = ORIENTED_EDGE ( 'NONE', *, *, #2525, .T. ) ;
#4107 =( CONVERSION_BASED_UNIT ( 'INCH', #57 ) LENGTH_UNIT ( ) NAMED_UNIT ( #5848 ) );
#4108 = FACE_OUTER_BOUND ( 'NONE', #7290, .T. ) ;
#4109 = DIRECTION ( 'NONE',  ( -0.000000000000000000, -0.000000000000000000, 1.000000000000000000 ) ) ;
#4110 = CARTESIAN_POINT ( 'NONE',  ( 0.3387180295041032907, -0.02886098700874997411, -0.2952755905511810219 ) ) ;
#4111 = ADVANCED_FACE ( 'NONE', ( #3917 ), #6688, .T. ) ;
#4112 = EDGE_CURVE ( 'NONE', #3843, #210, #6206, .T. ) ;
#4113 = AXIS2_PLACEMENT_3D ( 'NONE', #4362, #5560, #318 ) ;
#4114 = CARTESIAN_POINT ( 'NONE',  ( -0.02898191724071506881, -0.3924131423350828429, -0.3862808132025621344 ) ) ;
#4115 = CARTESIAN_POINT ( 'NONE',  ( 0.4466264210910796950, -0.9159926810392086116, -1.451746030331783510 ) ) ;
#4116 = DIRECTION ( 'NONE',  ( 0.000000000000000000, 1.000000000000000000, 0.000000000000000000 ) ) ;
#4117 = ITEM_DEFINED_TRANSFORMATION ( 'NONE', 'NONE', #5714,  #5166 ) ;
#4118 = AXIS2_PLACEMENT_3D ( 'NONE', #2781, #5006, #6801 ) ;
#4119 = CARTESIAN_POINT ( 'NONE',  ( 0.3581828924050323715, -0.1743168766271109560, 0.3019256869348722616 ) ) ;
#4120 = ORIENTED_EDGE ( 'NONE', *, *, #6602, .F. ) ;
#4121 = CARTESIAN_POINT ( 'NONE',  ( -0.4330708661417317362, -1.048552902599920955, -1.573978973432617279 ) ) ;
#4122 = DIRECTION ( 'NONE',  ( -1.000000000000000000, -0.000000000000000000, -0.000000000000000000 ) ) ;
#4123 = ORIENTED_EDGE ( 'NONE', *, *, #4669, .T. ) ;
#4124 = B_SPLINE_CURVE_WITH_KNOTS ( 'NONE', 3,
 ( #2438, #6080, #6612, #6006, #3121, #722 ),
 .UNSPECIFIED., .F., .F.,
 ( 4, 2, 4 ),
 ( 0.02186578511398849095, 0.02405896738650913774, 0.02625214965902978106 ),
 .UNSPECIFIED. ) ;
#4125 = ORIENTED_EDGE ( 'NONE', *, *, #5490, .T. ) ;
#4126 = CARTESIAN_POINT ( 'NONE',  ( 0.3528999085283635040, 0.1454870853231265693, 0.3018102362147644380 ) ) ;
#4127 = DIRECTION ( 'NONE',  ( 0.000000000000000000, -1.000000000000000000, 0.000000000000000000 ) ) ;
#4128 = ORIENTED_EDGE ( 'NONE', *, *, #3501, .T. ) ;
#4129 = AXIS2_PLACEMENT_3D ( 'NONE', #564, #3393, #1667 ) ;
#4130 = DIRECTION ( 'NONE',  ( 0.000000000000000000, 0.000000000000000000, -1.000000000000000000 ) ) ;
#4131 = CYLINDRICAL_SURFACE ( 'NONE', #2675, 0.2362204724409448231 ) ;
#4132 = LINE ( 'NONE', #1722, #3289 ) ;
#4133 = VERTEX_POINT ( 'NONE', #6896 ) ;
#4134 = FACE_OUTER_BOUND ( 'NONE', #6958, .T. ) ;
#4135 = CIRCLE ( 'NONE', #6458, 1.377952755905511806 ) ;
#4136 = CARTESIAN_POINT ( 'NONE',  ( 0.3322368487464851805, -0.06186759433717738121, 0.2952755905511811330 ) ) ;
#4137 = DIRECTION ( 'NONE',  ( 0.000000000000000000, 0.000000000000000000, 1.000000000000000000 ) ) ;
#4138 = CARTESIAN_POINT ( 'NONE',  ( 0.3409809061799574659, 0.02876216262209277050, 0.3014914394333951253 ) ) ;
#4139 = VERTEX_POINT ( 'NONE', #2759 ) ;
#4140 = CARTESIAN_POINT ( 'NONE',  ( -1.060348472569314193, -0.4341579012690721662, -1.570964862939435269 ) ) ;
#4141 = B_SPLINE_CURVE_WITH_KNOTS ( 'NONE', 3,
 ( #1945, #159, #6577, #5437, #194, #687 ),
 .UNSPECIFIED., .F., .F.,
 ( 4, 2, 4 ),
 ( 2.380732026380572752E-07, 0.002190927868076664002, 0.004381617662950689981 ),
 .UNSPECIFIED. ) ;
#4142 = AXIS2_PLACEMENT_3D ( 'NONE', #4887, #1906, #5345 ) ;
#4143 = CARTESIAN_POINT ( 'NONE',  ( -0.7480314960629922405, 1.220472440944881942, 2.952755905511811108 ) ) ;
#4144 = EDGE_LOOP ( 'NONE', ( #3671, #6143, #6889 ) ) ;
#4145 = TOROIDAL_SURFACE ( 'NONE', #1584, 1.043121362164705745, 0.05905511811023622659 ) ;
#4146 = EDGE_CURVE ( 'NONE', #2327, #7237, #4366, .T. ) ;
#4147 = CARTESIAN_POINT ( 'NONE',  ( 0.3543307086614173040, 0.06965032677943210071, -0.003053646640237114764 ) ) ;
#4148 = CARTESIAN_POINT ( 'NONE',  ( -1.048552902599921843, 0.4330708661417285721, -1.573978973432616835 ) ) ;
#4149 = FACE_OUTER_BOUND ( 'NONE', #434, .T. ) ;
#4150 = CARTESIAN_POINT ( 'NONE',  ( 0.000000000000000000, 0.000000000000000000, 0.2362204724409449064 ) ) ;
#4151 = CARTESIAN_POINT ( 'NONE',  ( -1.126887297386508504E-15, -0.4091458600556405756, -0.3766201741223081378 ) ) ;
#4152 = CARTESIAN_POINT ( 'NONE',  ( 0.4685039370078740717, -0.3409548833797009237, 0.000000000000000000 ) ) ;
#4153 = CARTESIAN_POINT ( 'NONE',  ( 1.850393700787401619, 0.7480314960629921295, 0.7480314960629921295 ) ) ;
#4154 = EDGE_CURVE ( 'NONE', #4931, #4654, #123, .T. ) ;
#4155 = EDGE_CURVE ( 'NONE', #1762, #5092, #4784, .T. ) ;
#4156 = CARTESIAN_POINT ( 'NONE',  ( 1.078368654584398456, 0.4878048847236929331, -1.510181419419387439 ) ) ;
#4157 = CIRCLE ( 'NONE', #3306, 0.4921259842519685179 ) ;
#4158 = DIRECTION ( 'NONE',  ( 0.000000000000000000, 0.000000000000000000, -1.000000000000000000 ) ) ;
#4159 = CARTESIAN_POINT ( 'NONE',  ( 0.3581828924050324825, 0.3486337532542225226, 1.056976728655274672E-17 ) ) ;
#4160 = CARTESIAN_POINT ( 'NONE',  ( 0.002549129251874865387, 0.05807386165059042621, 0.2952755905511811330 ) ) ;
#4161 = DIRECTION ( 'NONE',  ( -1.000000000000000000, -0.000000000000000000, -0.000000000000000000 ) ) ;
#4162 = ORIENTED_EDGE ( 'NONE', *, *, #3938, .T. ) ;
#4163 = CARTESIAN_POINT ( 'NONE',  ( 0.3581828924050323715, 0.1743168766271107895, -0.3019256869348722061 ) ) ;
#4164 = EDGE_CURVE ( 'NONE', #6698, #813, #5316, .T. ) ;
#4165 = DIRECTION ( 'NONE',  ( -0.000000000000000000, -0.000000000000000000, 1.000000000000000000 ) ) ;
#4166 = VERTEX_POINT ( 'NONE', #578 ) ;
#4167 = AXIS2_PLACEMENT_3D ( 'NONE', #59, #6484, #1230 ) ;
#4168 = ORIENTED_EDGE ( 'NONE', *, *, #6125, .F. ) ;
#4169 = CARTESIAN_POINT ( 'NONE',  ( 7.874015748031496287, 0.000000000000000000, 0.4921259842519685179 ) ) ;
#4170 = CARTESIAN_POINT ( 'NONE',  ( 1.968503937007874072, 1.496062992125984259, 0.000000000000000000 ) ) ;
#4171 = AXIS2_PLACEMENT_3D ( 'NONE', #908, #3236, #337 ) ;
#4172 = VERTEX_POINT ( 'NONE', #4059 ) ;
#4173 =( GEOMETRIC_REPRESENTATION_CONTEXT ( 3 ) GLOBAL_UNCERTAINTY_ASSIGNED_CONTEXT ( ( #6042 ) ) GLOBAL_UNIT_ASSIGNED_CONTEXT ( ( #4107, #3993, #6943 ) ) REPRESENTATION_CONTEXT ( 'NONE', 'WORKASPACE' ) );
#4174 = CARTESIAN_POINT ( 'NONE',  ( 0.4843361811957743734, 0.9895437626941967491, -1.389133361342958173 ) ) ;
#4175 = AXIS2_PLACEMENT_3D ( 'NONE', #4220, #2567, #5363 ) ;
#4176 = EDGE_LOOP ( 'NONE', ( #5540, #5717, #4024, #6414 ) ) ;
#4177 = AXIS2_PLACEMENT_3D ( 'NONE', #5920, #6445, #1193 ) ;
#4178 = CARTESIAN_POINT ( 'NONE',  ( 0.3531511627980769008, -0.3349346966101605649, -0.02350890366535178522 ) ) ;
#4179 = CARTESIAN_POINT ( 'NONE',  ( 0.000000000000000000, 1.496062992125984259, 0.000000000000000000 ) ) ;
#4180 = DIRECTION ( 'NONE',  ( 1.000000000000000000, 0.000000000000000000, 0.000000000000000000 ) ) ;
#4181 = CARTESIAN_POINT ( 'NONE',  ( 0.000000000000000000, 2.957312202238506242E-17, 0.2952755905511810774 ) ) ;
#4182 = DIRECTION ( 'NONE',  ( 1.000000000000000000, 0.000000000000000000, 0.000000000000000000 ) ) ;
#4183 = CARTESIAN_POINT ( 'NONE',  ( 0.000000000000000000, 0.000000000000000000, 0.000000000000000000 ) ) ;
#4184 = EDGE_LOOP ( 'NONE', ( #3979, #5369 ) ) ;
#4185 = CIRCLE ( 'NONE', #6031, 1.168853328413307135 ) ;
#4186 = DIRECTION ( 'NONE',  ( 1.000000000000000000, 0.000000000000000000, 0.000000000000000000 ) ) ;
#4187 = ORIENTED_EDGE ( 'NONE', *, *, #5052, .F. ) ;
#4188 =( CONVERSION_BASED_UNIT ( 'INCH', #1507 ) LENGTH_UNIT ( ) NAMED_UNIT ( #6920 ) );
#4189 = AXIS2_PLACEMENT_3D ( 'NONE', #4686, #2429, #5263 ) ;
#4190 = CARTESIAN_POINT ( 'NONE',  ( 0.3388536909603144798, -0.2250264928541644005, -0.2007938624299156205 ) ) ;
#4191 = CARTESIAN_POINT ( 'NONE',  ( 1.044891351410285552, 0.4330708661417424499, -1.574550377471545470 ) ) ;
#4192 = PRESENTATION_STYLE_ASSIGNMENT (( #1231 ) ) ;
#4193 = CARTESIAN_POINT ( 'NONE',  ( -1.279527559055117836, 1.968503937007873850, 2.480314960629921295 ) ) ;
#4194 = PRODUCT_DEFINITION_CONTEXT ( 'detailed design', #4039, 'design' ) ;
#4195 = DIRECTION ( 'NONE',  ( 0.000000000000000000, 0.000000000000000000, -1.000000000000000000 ) ) ;
#4196 = CARTESIAN_POINT ( 'NONE',  ( 0.9783381746514221433, 0.4342019027940302034, -1.450123259817210908 ) ) ;
#4197 = CARTESIAN_POINT ( 'NONE',  ( 2.755905511811024056, 1.496062992125984259, 0.000000000000000000 ) ) ;
#4198 = ITEM_DEFINED_TRANSFORMATION ( 'NONE', 'NONE', #4712,  #5166 ) ;
#4199 = CARTESIAN_POINT ( 'NONE',  ( 0.000000000000000000, 0.000000000000000000, -0.4082677165354330340 ) ) ;
#4200 = FACE_OUTER_BOUND ( 'NONE', #4620, .T. ) ;
#4201 = CARTESIAN_POINT ( 'NONE',  ( 0.000000000000000000, 0.000000000000000000, -1.484898342931014303 ) ) ;
#4202 = DIRECTION ( 'NONE',  ( 0.000000000000000000, 0.000000000000000000, -1.000000000000000000 ) ) ;
#4203 = ORIENTED_EDGE ( 'NONE', *, *, #2655, .T. ) ;
#4204 = CLOSED_SHELL ( 'NONE', ( #1111, #204, #4446, #4399, #6444, #4851, #39, #7329, #1345, #5835, #5993, #1685, #5326, #6448, #5845, #5892, #4811, #1397, #4776, #4547, #852, #3132, #6037, #5585, #7006, #3327, #7143, #1801, #2281 ) ) ;
#4205 = CARTESIAN_POINT ( 'NONE',  ( -0.2362204724409449619, 0.000000000000000000, -0.4072677165354330331 ) ) ;
#4206 = CARTESIAN_POINT ( 'NONE',  ( 0.000000000000000000, 0.000000000000000000, 0.000000000000000000 ) ) ;
#4207 = EDGE_CURVE ( 'NONE', #6087, #7025, #4980, .T. ) ;
#4208 = ADVANCED_FACE ( 'NONE', ( #5857 ), #1252, .F. ) ;
#4209 = ORIENTED_EDGE ( 'NONE', *, *, #2525, .F. ) ;
#4210 = CARTESIAN_POINT ( 'NONE',  ( 0.7480314960629922405, 1.220472440944881942, 0.000000000000000000 ) ) ;
#4211 = EDGE_CURVE ( 'NONE', #7286, #5092, #6811, .T. ) ;
#4212 = DIRECTION ( 'NONE',  ( 1.000000000000000000, 0.000000000000000000, 0.000000000000000000 ) ) ;
#4213 = ORIENTED_EDGE ( 'NONE', *, *, #389, .F. ) ;
#4214 = CARTESIAN_POINT ( 'NONE',  ( 0.4330708661417321803, 0.9697097892794909191, -1.453662943332485247 ) ) ;
#4215 = B_SPLINE_CURVE_WITH_KNOTS ( 'NONE', 3,
 ( #4070, #2875, #497, #3428, #7502, #2272, #6400, #1144 ),
 .UNSPECIFIED., .F., .F.,
 ( 4, 2, 2, 4 ),
 ( 0.005257893453559884557, 0.006567392922673222569, 0.007876892391786559713, 0.01049589133001323574 ),
 .UNSPECIFIED. ) ;
#4216 = EDGE_CURVE ( 'NONE', #1378, #5614, #1550, .T. ) ;
#4217 = ADVANCED_FACE ( 'NONE', ( #6463 ), #2979, .T. ) ;
#4218 = ORIENTED_EDGE ( 'NONE', *, *, #2847, .F. ) ;
#4219 = EDGE_LOOP ( 'NONE', ( #7176, #3947, #965, #7160 ) ) ;
#4220 = CARTESIAN_POINT ( 'NONE',  ( 0.000000000000000000, 0.2559055118110236116, 0.000000000000000000 ) ) ;
#4221 = CARTESIAN_POINT ( 'NONE',  ( -0.2371576072764295939, 0.2722228516542259391, -0.4052515342986937608 ) ) ;
#4222 = PRODUCT_CONTEXT ( 'NONE', #6055, 'mechanical' ) ;
#4223 = DIRECTION ( 'NONE',  ( 1.000000000000000000, 0.000000000000000000, -0.000000000000000000 ) ) ;
#4224 = ORIENTED_EDGE ( 'NONE', *, *, #1483, .F. ) ;
#4225 = VERTEX_POINT ( 'NONE', #7118 ) ;
#4226 = EDGE_LOOP ( 'NONE', ( #990, #354, #5447, #3048, #5561 ) ) ;
#4227 =( LENGTH_UNIT ( ) NAMED_UNIT ( * ) SI_UNIT ( $, .METRE. ) );
#4228 = PRODUCT_DEFINITION_SHAPE ( 'NONE', 'NONE',  #7526 ) ;
#4229 = DIRECTION ( 'NONE',  ( -1.000000000000000000, 0.000000000000000000, 0.000000000000000000 ) ) ;
#4230 = CARTESIAN_POINT ( 'NONE',  ( 0.7690174846032691303, -0.09763972085202782258, -0.9794230103293317669 ) ) ;
#4231 = AXIS2_PLACEMENT_3D ( 'NONE', #6329, #5153, #2735 ) ;
#4232 = CARTESIAN_POINT ( 'NONE',  ( 0.5072022184710041071, -1.064268091466991084, -1.491294347567119427 ) ) ;
#4233 = DIRECTION ( 'NONE',  ( 1.000000000000000000, 0.000000000000000000, -0.000000000000000000 ) ) ;
#4234 = CARTESIAN_POINT ( 'NONE',  ( 0.3391892065151629332, 0.1988903486381583818, 0.2460629921259842312 ) ) ;
#4235 = CARTESIAN_POINT ( 'NONE',  ( 0.000000000000000000, 0.000000000000000000, -0.4082677165354330340 ) ) ;
#4236 = CARTESIAN_POINT ( 'NONE',  ( 1.080458355692609729, 0.4837911690062530745, -1.514208178040841846 ) ) ;
#4237 = CARTESIAN_POINT ( 'NONE',  ( 0.000000000000000000, 0.2559055118110236116, -0.4921259842519685179 ) ) ;
#4238 = DIRECTION ( 'NONE',  ( 1.000000000000000000, 0.000000000000000000, 2.095133389269358970E-15 ) ) ;
#4239 = CARTESIAN_POINT ( 'NONE',  ( -0.4338950423154138147, 1.037563309807725043, -1.574803149606299302 ) ) ;
#4240 = DIRECTION ( 'NONE',  ( -0.5000000000000008882, 0.8660254037844381525, 0.000000000000000000 ) ) ;
#4241 = ORIENTED_EDGE ( 'NONE', *, *, #6733, .F. ) ;
#4242 = CARTESIAN_POINT ( 'NONE',  ( -0.9810555383103384264, 0.4349192646538826978, -1.448591292758282245 ) ) ;
#4243 = FACE_BOUND ( 'NONE', #5854, .T. ) ;
#4244 = ORIENTED_EDGE ( 'NONE', *, *, #4246, .T. ) ;
#4245 = FACE_OUTER_BOUND ( 'NONE', #4555, .T. ) ;
#4246 = EDGE_CURVE ( 'NONE', #655, #6508, #7044, .T. ) ;
#4247 = CARTESIAN_POINT ( 'NONE',  ( 0.4332776171645018048, 1.054581729003112311, -1.572814845875644352 ) ) ;
#4248 = ORIENTED_EDGE ( 'NONE', *, *, #5233, .T. ) ;
#4249 = DIRECTION ( 'NONE',  ( 1.000000000000000000, 0.000000000000000000, -0.000000000000000000 ) ) ;
#4250 = AXIS2_PLACEMENT_3D ( 'NONE', #7409, #2749, #5639 ) ;
#4251 = ORIENTED_EDGE ( 'NONE', *, *, #6837, .T. ) ;
#4252 = ORIENTED_EDGE ( 'NONE', *, *, #5431, .F. ) ;
#4253 = CARTESIAN_POINT ( 'NONE',  ( 0.000000000000000000, 1.496062992125984259, -0.2362204724409449341 ) ) ;
#4254 = CONTEXT_DEPENDENT_SHAPE_REPRESENTATION ( #1692, #874 ) ;
#4255 = CIRCLE ( 'NONE', #6333, 1.168853328413307135 ) ;
#4256 = EDGE_CURVE ( 'NONE', #4277, #3423, #3507, .T. ) ;
#4257 = FILL_AREA_STYLE ('',( #1928 ) ) ;
#4258 = ORIENTED_EDGE ( 'NONE', *, *, #943, .F. ) ;
#4259 = EDGE_CURVE ( 'NONE', #7070, #2864, #1210, .T. ) ;
#4260 = CARTESIAN_POINT ( 'NONE',  ( 0.3565422412058069090, 0.1767728485866832400, 0.2952755905511811330 ) ) ;
#4261 = CARTESIAN_POINT ( 'NONE',  ( 1.083679028610385009, -0.4756000659977862588, -1.522578585053779188 ) ) ;
#4262 = ORIENTED_EDGE ( 'NONE', *, *, #6957, .F. ) ;
#4263 = CARTESIAN_POINT ( 'NONE',  ( 1.718248690375545225E-15, -0.4921259842519648542, -2.204724409448822975 ) ) ;
#4264 = AXIS2_PLACEMENT_3D ( 'NONE', #3442, #3406, #1678 ) ;
#4265 = ORIENTED_EDGE ( 'NONE', *, *, #4105, .T. ) ;
#4266 = CARTESIAN_POINT ( 'NONE',  ( -0.4700904924197908397, 0.8785537298370134085, -1.433776001880364470 ) ) ;
#4267 = FILL_AREA_STYLE ('',( #3114 ) ) ;
#4268 = CIRCLE ( 'NONE', #6226, 1.168853328413308690 ) ;
#4269 = FACE_OUTER_BOUND ( 'NONE', #5678, .T. ) ;
#4270 = DIRECTION ( 'NONE',  ( 0.000000000000000000, 0.000000000000000000, -1.000000000000000000 ) ) ;
#4271 = CARTESIAN_POINT ( 'NONE',  ( 3.414809992080329023E-17, 0.4091458600556405201, -0.03164754241312491001 ) ) ;
#4272 = CARTESIAN_POINT ( 'NONE',  ( 1.054581729003108759, 0.4332776171645121299, -1.572814845875644352 ) ) ;
#4273 = CARTESIAN_POINT ( 'NONE',  ( 0.000000000000000000, 0.000000000000000000, 0.000000000000000000 ) ) ;
#4274 = CARTESIAN_POINT ( 'NONE',  ( -0.3254211578371894453, -0.2212638669783398016, -0.02201102547170743703 ) ) ;
#4275 = CARTESIAN_POINT ( 'NONE',  ( 0.3543307086614173596, -0.1713008003332313622, -0.3862250106401512451 ) ) ;
#4276 = DIRECTION ( 'NONE',  ( 0.000000000000000000, 0.000000000000000000, 1.000000000000000000 ) ) ;
#4277 = VERTEX_POINT ( 'NONE', #731 ) ;
#4278 = CARTESIAN_POINT ( 'NONE',  ( -0.9773781006402579852, 0.4999740374263504372, -1.373989084483999257 ) ) ;
#4279 = DIRECTION ( 'NONE',  ( 0.000000000000000000, 0.000000000000000000, 1.000000000000000000 ) ) ;
#4280 = CARTESIAN_POINT ( 'NONE',  ( 0.2952755905511811885, 3.616083068348484413E-17, -0.7983802283864783744 ) ) ;
#4281 = VECTOR ( 'NONE', #6457, 39.37007874015748143 ) ;
#4282 = DIRECTION ( 'NONE',  ( 0.000000000000000000, -1.000000000000000000, 0.000000000000000000 ) ) ;
#4283 = DIRECTION ( 'NONE',  ( 0.000000000000000000, 0.000000000000000000, 1.000000000000000000 ) ) ;
#4284 = ORIENTED_EDGE ( 'NONE', *, *, #2388, .F. ) ;
#4285 = FACE_OUTER_BOUND ( 'NONE', #4912, .T. ) ;
#4286 = AXIS2_PLACEMENT_3D ( 'NONE', #1030, #3437, #5778 ) ;
#4287 = ORIENTED_EDGE ( 'NONE', *, *, #1919, .T. ) ;
#4288 = PRODUCT_DEFINITION_SHAPE ( 'NONE', 'NONE',  #7533 ) ;
#4289 = EDGE_CURVE ( 'NONE', #1079, #7462, #4499, .T. ) ;
#4290 = VERTEX_POINT ( 'NONE', #3557 ) ;
#4291 = DIRECTION ( 'NONE',  ( -1.000000000000000000, 0.000000000000000000, 0.000000000000000000 ) ) ;
#4292 = CARTESIAN_POINT ( 'NONE',  ( 0.3561390657006787142, -0.3446602609999988021, 5.012419073868498717E-17 ) ) ;
#4293 = VERTEX_POINT ( 'NONE', #1135 ) ;
#4294 = CARTESIAN_POINT ( 'NONE',  ( 0.3487102105009254327, 0.3201373431253348167, 0.04891434758976444946 ) ) ;
#4295 = ORIENTED_EDGE ( 'NONE', *, *, #2715, .F. ) ;
#4296 = CIRCLE ( 'NONE', #3446, 0.2066929133858267931 ) ;
#4297 = CARTESIAN_POINT ( 'NONE',  ( 0.9227869198894881331, 0.2286038407206694989, 0.9573410596537438311 ) ) ;
#4298 = EDGE_LOOP ( 'NONE', ( #3786, #934, #4700 ) ) ;
#4299 = CARTESIAN_POINT ( 'NONE',  ( 0.000000000000000000, 0.000000000000000000, 0.1783464566929134354 ) ) ;
#4300 = DIRECTION ( 'NONE',  ( 0.000000000000000000, 1.000000000000000000, 0.000000000000000000 ) ) ;
#4301 = AXIS2_PLACEMENT_3D ( 'NONE', #2953, #4104, #2381 ) ;
#4302 = AXIS2_PLACEMENT_3D ( 'NONE', #2981, #2938, #7150 ) ;
#4303 = EDGE_CURVE ( 'NONE', #3366, #1484, #4699, .T. ) ;
#4304 = VERTEX_POINT ( 'NONE', #6422 ) ;
#4305 = EDGE_CURVE ( 'NONE', #733, #4592, #2005, .T. ) ;
#4306 =( NAMED_UNIT ( * ) SI_UNIT ( $, .STERADIAN. ) SOLID_ANGLE_UNIT ( ) );
#4307 = ADVANCED_FACE ( 'NONE', ( #1715 ), #6435, .T. ) ;
#4308 = DIRECTION ( 'NONE',  ( 0.8191520442889907994, 1.003171929053523514E-16, -0.5735764363510474917 ) ) ;
#4309 = DIRECTION ( 'NONE',  ( 1.000000000000000000, 0.000000000000000000, 0.000000000000000000 ) ) ;
#4310 = VECTOR ( 'NONE', #989, 39.37007874015748143 ) ;
#4311 = DIRECTION ( 'NONE',  ( 0.000000000000000000, 0.000000000000000000, -1.000000000000000000 ) ) ;
#4312 = EDGE_CURVE ( 'NONE', #7325, #7262, #2893, .T. ) ;
#4313 = AXIS2_PLACEMENT_3D ( 'NONE', #6796, #5158, #6755 ) ;
#4314 = DIRECTION ( 'NONE',  ( -1.000000000000000000, 0.000000000000000000, 0.000000000000000000 ) ) ;
#4315 = CARTESIAN_POINT ( 'NONE',  ( 0.3432736861146659657, 0.1420645347415416815, 0.2952755905511811330 ) ) ;
#4316 = DIRECTION ( 'NONE',  ( 0.000000000000000000, 0.000000000000000000, -1.000000000000000000 ) ) ;
#4317 = CARTESIAN_POINT ( 'NONE',  ( 0.000000000000000000, 1.496062992125984259, 0.7480314960629921295 ) ) ;
#4318 = CARTESIAN_POINT ( 'NONE',  ( 0.3391892065151631552, -0.1988903486381589925, -0.2460629921259842035 ) ) ;
#4319 = CARTESIAN_POINT ( 'NONE',  ( 0.3410425348215775920, 0.2462961272004790259, 0.1763890642357578975 ) ) ;
#4320 = CARTESIAN_POINT ( 'NONE',  ( 0.000000000000000000, 0.000000000000000000, -2.204724409448820754 ) ) ;
#4321 = DIRECTION ( 'NONE',  ( 0.000000000000000000, 0.000000000000000000, -1.000000000000000000 ) ) ;
#4322 = ORIENTED_EDGE ( 'NONE', *, *, #2161, .T. ) ;
#4323 = CARTESIAN_POINT ( 'NONE',  ( -0.9783380834473015542, 0.4342018836190565390, -1.450123305573143284 ) ) ;
#4324 = CARTESIAN_POINT ( 'NONE',  ( -0.4630671888207402165, 1.085749034841582139, -1.535808138920397026 ) ) ;
#4325 = MECHANICAL_DESIGN_GEOMETRIC_PRESENTATION_REPRESENTATION (  '', ( #6036 ), #7248 ) ;
#4326 = ORIENTED_EDGE ( 'NONE', *, *, #7279, .T. ) ;
#4327 = FACE_OUTER_BOUND ( 'NONE', #3942, .T. ) ;
#4328 = CARTESIAN_POINT ( 'NONE',  ( -0.5118110236220474452, 1.220472440944881942, 2.480314960629921295 ) ) ;
#4329 = CARTESIAN_POINT ( 'NONE',  ( 0.4330708661417322913, 0.9666437042230126009, -1.454455828411335583 ) ) ;
#4330 = ORIENTED_EDGE ( 'NONE', *, *, #5850, .F. ) ;
#4331 = CARTESIAN_POINT ( 'NONE',  ( 0.3398312250857988270, 0.1962691648278992451, -0.2506030156613296422 ) ) ;
#4332 = ORIENTED_EDGE ( 'NONE', *, *, #1471, .F. ) ;
#4333 = CIRCLE ( 'NONE', #5303, 0.2362204724409449064 ) ;
#4334 = EDGE_LOOP ( 'NONE', ( #4128, #4248, #3287, #4295 ) ) ;
#4335 = CARTESIAN_POINT ( 'NONE',  ( 0.3387177083556159873, -0.2701412011614057196, -0.1226528954731239129 ) ) ;
#4336 =( REPRESENTATION_RELATIONSHIP ('NONE','NONE', #303, #1307 ) REPRESENTATION_RELATIONSHIP_WITH_TRANSFORMATION ( #3905 )SHAPE_REPRESENTATION_RELATIONSHIP( ) );
#4337 = CARTESIAN_POINT ( 'NONE',  ( -1.037563309807726375, 0.4338950423154108171, -1.574803149606299302 ) ) ;
#4338 = CARTESIAN_POINT ( 'NONE',  ( 0.3496875272944829360, 0.3447318307381752600, -0.006541864722391422388 ) ) ;
#4339 = ORIENTED_EDGE ( 'NONE', *, *, #882, .T. ) ;
#4340 = CARTESIAN_POINT ( 'NONE',  ( 0.8401230830384029957, 0.1877837920673497696, 0.9662117393330279524 ) ) ;
#4341 = VERTEX_POINT ( 'NONE', #6697 ) ;
#4342 = DIRECTION ( 'NONE',  ( 1.000000000000000000, 0.000000000000000000, 0.000000000000000000 ) ) ;
#4343 = EDGE_LOOP ( 'NONE', ( #1999, #2269, #3768, #1782 ) ) ;
#4344 =( CONVERSION_BASED_UNIT ( 'INCH', #3155 ) LENGTH_UNIT ( ) NAMED_UNIT ( #3949 ) );
#4345 = CARTESIAN_POINT ( 'NONE',  ( 0.02637295201093697167, 0.1704774416898497680, -0.2952755905511810774 ) ) ;
#4346 = CARTESIAN_POINT ( 'NONE',  ( 1.220472440944881720, 1.984939871850715226E-17, -0.9842519685039370358 ) ) ;
#4347 = EDGE_CURVE ( 'NONE', #2144, #6423, #1167, .T. ) ;
#4348 = CARTESIAN_POINT ( 'NONE',  ( 0.4341579012690690575, -1.060348472569314415, -1.570964862939435491 ) ) ;
#4349 = DIRECTION ( 'NONE',  ( -1.000000000000000000, 0.000000000000000000, -0.000000000000000000 ) ) ;
#4350 = CARTESIAN_POINT ( 'NONE',  ( 0.3581828924050324825, -0.1743168766271116221, -0.3019256869348722061 ) ) ;
#4351 = EDGE_CURVE ( 'NONE', #3073, #3441, #1069, .T. ) ;
#4352 = CARTESIAN_POINT ( 'NONE',  ( 0.000000000000000000, 1.205361022782827973E-16, -0.9842519685039370358 ) ) ;
#4353 = ADVANCED_FACE ( 'NONE', ( #6017 ), #1374, .F. ) ;
#4354 = ORIENTED_EDGE ( 'NONE', *, *, #6966, .T. ) ;
#4355 = PRODUCT_DEFINITION_SHAPE ( 'NONE', 'NONE',  #7551 ) ;
#4356 = DIRECTION ( 'NONE',  ( -1.000000000000000000, -1.047067131017168686E-14, 0.000000000000000000 ) ) ;
#4357 = CARTESIAN_POINT ( 'NONE',  ( -0.4348450248026697884, 1.063161309294320178, -1.569784497862150463 ) ) ;
#4358 = CIRCLE ( 'NONE', #5353, 0.2362204724409448231 ) ;
#4359 = ORIENTED_EDGE ( 'NONE', *, *, #661, .F. ) ;
#4360 = CARTESIAN_POINT ( 'NONE',  ( 1.968503937007874072, 0.000000000000000000, 0.4921259842519685179 ) ) ;
#4361 = CARTESIAN_POINT ( 'NONE',  ( 0.02637295201093723881, -0.1704774416898505729, -0.2952755905511810774 ) ) ;
#4362 = CARTESIAN_POINT ( 'NONE',  ( 1.795185198899822598E-15, -0.5141614760841421994, -2.204724409448823419 ) ) ;
#4363 = ORIENTED_EDGE ( 'NONE', *, *, #7014, .T. ) ;
#4364 = CARTESIAN_POINT ( 'NONE',  ( 0.4368378848980529749, -1.023372273685339895, -1.573834172653142627 ) ) ;
#4365 = ORIENTED_EDGE ( 'NONE', *, *, #4718, .F. ) ;
#4366 = CIRCLE ( 'NONE', #583, 1.259842519685039131 ) ;
#4367 = ORIENTED_EDGE ( 'NONE', *, *, #7340, .T. ) ;
#4368 = CARTESIAN_POINT ( 'NONE',  ( 0.9842519685039370358, 0.7480314960629921295, 0.000000000000000000 ) ) ;
#4369 = B_SPLINE_CURVE_WITH_KNOTS ( 'NONE', 3,
 ( #4002, #1582, #7395, #2306, #4607, #4640, #3967, #7430, #1050, #6258 ),
 .UNSPECIFIED., .F., .F.,
 ( 4, 2, 2, 2, 4 ),
 ( 0.000000000000000000, 0.0005216184974661230425, 0.001043236994932246085, 0.001564855492398369019, 0.002086473989864492170 ),
 .UNSPECIFIED. ) ;
#4370 = FILL_AREA_STYLE ('',( #3145 ) ) ;
#4371 = ORIENTED_EDGE ( 'NONE', *, *, #6696, .T. ) ;
#4372 = CARTESIAN_POINT ( 'NONE',  ( 0.9960021845704909449, -0.4720891361949376419, -1.401719468380311140 ) ) ;
#4373 = ORIENTED_EDGE ( 'NONE', *, *, #4764, .F. ) ;
#4374 = AXIS2_PLACEMENT_3D ( 'NONE', #723, #6047, #4929 ) ;
#4375 = CARTESIAN_POINT ( 'NONE',  ( 0.3391892065151629332, 0.1136516277932330399, -0.2952755905511810774 ) ) ;
#4376 = ORIENTED_EDGE ( 'NONE', *, *, #2620, .F. ) ;
#4377 = CARTESIAN_POINT ( 'NONE',  ( 0.3496875272944829360, 0.3447318307381752600, -0.006541864722391422388 ) ) ;
#4378 = ORIENTED_EDGE ( 'NONE', *, *, #2754, .T. ) ;
#4379 = ORIENTED_EDGE ( 'NONE', *, *, #2246, .T. ) ;
#4380 = TOROIDAL_SURFACE ( 'NONE', #1313, 1.223643328182682621, 0.05905511811023622659 ) ;
#4381 = DIRECTION ( 'NONE',  ( 0.000000000000000000, 0.000000000000000000, -1.000000000000000000 ) ) ;
#4382 = DIRECTION ( 'NONE',  ( -0.000000000000000000, -0.000000000000000000, 1.000000000000000000 ) ) ;
#4383 = CARTESIAN_POINT ( 'NONE',  ( 0.9997522001112967294, -0.2362259618796917759, -0.9554837688155867204 ) ) ;
#4384 = CIRCLE ( 'NONE', #5238, 0.2362204724409449341 ) ;
#4385 = CARTESIAN_POINT ( 'NONE',  ( -0.9411659768779426782, -0.4368170415251763639, -1.456692913385828847 ) ) ;
#4386 = CARTESIAN_POINT ( 'NONE',  ( 1.015186846506429985, 0.2347025779575657722, -0.9558642380754210910 ) ) ;
#4387 = EDGE_CURVE ( 'NONE', #614, #5178, #2538, .T. ) ;
#4388 = DIRECTION ( 'NONE',  ( -1.000000000000000000, 0.000000000000000000, 0.000000000000000000 ) ) ;
#4389 = AXIS2_PLACEMENT_3D ( 'NONE', #3046, #2482, #4815 ) ;
#4390 = CARTESIAN_POINT ( 'NONE',  ( 0.4627498550472184946, 0.8884031170519962606, -1.439912866901231547 ) ) ;
#4391 = LINE ( 'NONE', #6686, #2291 ) ;
#4392 = DIRECTION ( 'NONE',  ( -0.000000000000000000, -0.000000000000000000, 1.000000000000000000 ) ) ;
#4393 = ORIENTED_EDGE ( 'NONE', *, *, #5374, .T. ) ;
#4394 = CARTESIAN_POINT ( 'NONE',  ( -0.9867938558989117759, 0.4882975260543697682, -1.385219839936550956 ) ) ;
#4395 = CIRCLE ( 'NONE', #3915, 0.4507874015748032370 ) ;
#4396 = ORIENTED_EDGE ( 'NONE', *, *, #4861, .F. ) ;
#4397 = DIRECTION ( 'NONE',  ( -1.000000000000000000, 0.000000000000000000, 0.000000000000000000 ) ) ;
#4398 = EDGE_CURVE ( 'NONE', #2106, #4444, #1556, .T. ) ;
#4399 = ADVANCED_FACE ( 'NONE', ( #1916 ), #4940, .T. ) ;
#4400 = CARTESIAN_POINT ( 'NONE',  ( 0.3997746709170348356, 5.668966274263039413E-17, 0.4629062255509093782 ) ) ;
#4401 = APPLICATION_PROTOCOL_DEFINITION ( 'draft international standard', 'automotive_design', 1998, #915 ) ;
#4402 = CARTESIAN_POINT ( 'NONE',  ( 3.414809992080329023E-17, 0.4091458600556405201, -0.03164754241312491001 ) ) ;
#4403 = ORIENTED_EDGE ( 'NONE', *, *, #4246, .F. ) ;
#4404 = CYLINDRICAL_SURFACE ( 'NONE', #535, 0.2362204724409449619 ) ;
#4405 = B_SPLINE_CURVE_WITH_KNOTS ( 'NONE', 3,
 ( #6980, #537, #502, #5805, #4040, #7506, #6373, #3468, #1591, #4684 ),
 .UNSPECIFIED., .F., .F.,
 ( 4, 2, 2, 2, 4 ),
 ( 6.564673817405236669E-19, 0.002239656411828510989, 0.004479312823657021110, 0.006718969235485531231, 0.008958625647314040485 ),
 .UNSPECIFIED. ) ;
#4406 = ORIENTED_EDGE ( 'NONE', *, *, #6264, .F. ) ;
#4407 = ORIENTED_EDGE ( 'NONE', *, *, #4112, .F. ) ;
#4408 = DIRECTION ( 'NONE',  ( -0.000000000000000000, -0.000000000000000000, 1.000000000000000000 ) ) ;
#4409 = LINE ( 'NONE', #5569, #6452 ) ;
#4410 = VERTEX_POINT ( 'NONE', #4402 ) ;
#4411 = AXIS2_PLACEMENT_3D ( 'NONE', #611, #6580, #2400 ) ;
#4412 = CARTESIAN_POINT ( 'NONE',  ( 0.9079010304997725544, 0.2240813082648737964, 0.9584242268600799974 ) ) ;
#4413 = VERTEX_POINT ( 'NONE', #205 ) ;
#4414 =( LENGTH_UNIT ( ) NAMED_UNIT ( * ) SI_UNIT ( $, .METRE. ) );
#4415 = CARTESIAN_POINT ( 'NONE',  ( 0.000000000000000000, 0.000000000000000000, 0.000000000000000000 ) ) ;
#4416 = ORIENTED_EDGE ( 'NONE', *, *, #6446, .T. ) ;
#4417 = AXIS2_PLACEMENT_3D ( 'NONE', #7221, #1996, #4440 ) ;
#4418 = DIRECTION ( 'NONE',  ( 0.000000000000000000, 0.000000000000000000, 1.000000000000000000 ) ) ;
#4419 = PRODUCT_DEFINITION_SHAPE ( 'NONE', 'NONE',  #7530 ) ;
#4420 = DIRECTION ( 'NONE',  ( 1.000000000000000000, 0.000000000000000000, 0.000000000000000000 ) ) ;
#4421 = CARTESIAN_POINT ( 'NONE',  ( 0.3574269917172684941, -0.1732784665916271005, -0.3001271079943088615 ) ) ;
#4422 = DIRECTION ( 'NONE',  ( 0.000000000000000000, 0.000000000000000000, -1.000000000000000000 ) ) ;
#4423 = CARTESIAN_POINT ( 'NONE',  ( 0.7836514762968587178, -0.1249763776241986785, -0.9763066675542205752 ) ) ;
#4424 = CIRCLE ( 'NONE', #6626, 0.9964144355006141485 ) ;
#4425 =( GEOMETRIC_REPRESENTATION_CONTEXT ( 3 ) GLOBAL_UNCERTAINTY_ASSIGNED_CONTEXT ( ( #7050 ) ) GLOBAL_UNIT_ASSIGNED_CONTEXT ( ( #6262, #3972, #6797 ) ) REPRESENTATION_CONTEXT ( 'NONE', 'WORKASPACE' ) );
#4426 = FACE_OUTER_BOUND ( 'NONE', #1566, .T. ) ;
#4427 = CARTESIAN_POINT ( 'NONE',  ( 0.9998202959290236613, 0.2362140621487221481, -0.9554867107345892396 ) ) ;
#4428 = AXIS2_PLACEMENT_3D ( 'NONE', #7416, #3337, #966 ) ;
#4429 = TOROIDAL_SURFACE ( 'NONE', #1983, 1.223643328182682621, 0.05905511811023622659 ) ;
#4430 = DIRECTION ( 'NONE',  ( 0.000000000000000000, 1.000000000000000000, 2.193342766891360832E-15 ) ) ;
#4431 = DIRECTION ( 'NONE',  ( -0.000000000000000000, 0.8660254037844383745, 0.5000000000000006661 ) ) ;
#4432 = CARTESIAN_POINT ( 'NONE',  ( -0.4659838021914858852, 0.9705345056685065197, -1.550372027848314405 ) ) ;
#4433 = VERTEX_POINT ( 'NONE', #4976 ) ;
#4434 = FACE_OUTER_BOUND ( 'NONE', #357, .T. ) ;
#4435 = EDGE_CURVE ( 'NONE', #3477, #1882, #6649, .T. ) ;
#4436 = AXIS2_PLACEMENT_3D ( 'NONE', #5059, #1562, #3910 ) ;
#4437 = APPLICATION_CONTEXT ( 'automotive_design' ) ;
#4438 = ORIENTED_EDGE ( 'NONE', *, *, #6603, .F. ) ;
#4439 = CARTESIAN_POINT ( 'NONE',  ( 0.000000000000000000, 0.2557161625347750267, 0.1476377952755908163 ) ) ;
#4440 = DIRECTION ( 'NONE',  ( 0.000000000000000000, 0.000000000000000000, -1.000000000000000000 ) ) ;
#4441 = SHAPE_DEFINITION_REPRESENTATION ( #2997, #2912 ) ;
#4442 = AXIS2_PLACEMENT_3D ( 'NONE', #2812, #6870, #3312 ) ;
#4443 = CARTESIAN_POINT ( 'NONE',  ( 0.2371803407075527004, 0.2722097265016475420, -0.003642820150508603583 ) ) ;
#4444 = VERTEX_POINT ( 'NONE', #4897 ) ;
#4445 = CARTESIAN_POINT ( 'NONE',  ( 0.3585569128062319200, 0.3496569568119790028, 0.001755940978325809575 ) ) ;
#4446 = ADVANCED_FACE ( 'NONE', ( #2526 ), #5967, .T. ) ;
#4447 = EDGE_CURVE ( 'NONE', #5491, #6357, #457, .T. ) ;
#4448 = ORIENTED_EDGE ( 'NONE', *, *, #6050, .F. ) ;
#4449 = VERTEX_POINT ( 'NONE', #3679 ) ;
#4450 = EDGE_CURVE ( 'NONE', #5491, #5648, #3514, .T. ) ;
#4451 = AXIS2_PLACEMENT_3D ( 'NONE', #2916, #3355, #25 ) ;
#4452 = CARTESIAN_POINT ( 'NONE',  ( -1.320571051624814422E-17, -0.02882762270237488114, -0.2952755905511810219 ) ) ;
#4453 = DIRECTION ( 'NONE',  ( -1.000000000000000000, 0.000000000000000000, -0.000000000000000000 ) ) ;
#4454 =( BOUNDED_SURFACE ( )  B_SPLINE_SURFACE ( 3, 2, ( 
 ( #7162, #1932, #6600 ),
 ( #932, #6745, #3923 ),
 ( #7424, #2196, #407 ),
 ( #6142, #3877, #1532 ),
 ( #366, #1130, #3261 ),
 ( #7390, #6386, #2160 ),
 ( #6251, #6213, #1575 ),
 ( #4377, #2766, #4528 ) ),
 .UNSPECIFIED., .F., .F., .F. ) 
 B_SPLINE_SURFACE_WITH_KNOTS ( ( 4, 2, 2, 4 ),
 ( 3, 3 ),
 ( 0.03551798592901333346, 0.03994769179990642627, 0.04216254473535296921, 0.04437739767079951908 ),
 ( 0.000000000000000000, 1.000000000000000000 ),
 .UNSPECIFIED. ) 
 GEOMETRIC_REPRESENTATION_ITEM ( )  RATIONAL_B_SPLINE_SURFACE ( (
 ( 1.000000000000000000, 0.8047781103519391355, 1.000000000000000000),
 ( 1.000000000000000000, 0.8123785826169017676, 1.000000000000000000),
 ( 1.000000000000000000, 0.8190671539036440407, 1.000000000000000000),
 ( 1.000000000000000000, 0.8191932076449144340, 1.000000000000000000),
 ( 1.000000000000000000, 0.8176085094066379844, 1.000000000000000000),
 ( 1.000000000000000000, 0.8122955484014008354, 1.000000000000000000),
 ( 1.000000000000000000, 0.8086308001280846369, 1.000000000000000000),
 ( 1.000000000000000000, 0.8047712537969720081, 1.000000000000000000) ) ) 
 REPRESENTATION_ITEM ( '' )  SURFACE ( )  );
#4455 =( CONVERSION_BASED_UNIT ( 'INCH', #2121 ) LENGTH_UNIT ( ) NAMED_UNIT ( #6292 ) );
#4456 = VERTEX_POINT ( 'NONE', #5020 ) ;
#4457 = CARTESIAN_POINT ( 'NONE',  ( 0.3426144402834028768, 0.2904173629089201736, 0.1000635707556194326 ) ) ;
#4458 = ORIENTED_EDGE ( 'NONE', *, *, #7285, .F. ) ;
#4459 = CARTESIAN_POINT ( 'NONE',  ( 0.3543307086614172485, 0.000000000000000000, 0.3732633159281743551 ) ) ;
#4460 = EDGE_CURVE ( 'NONE', #1950, #5498, #1914, .T. ) ;
#4461 = EDGE_LOOP ( 'NONE', ( #1609, #2356 ) ) ;
#4462 = EDGE_CURVE ( 'NONE', #1296, #1000, #4551, .T. ) ;
#4463 = VERTEX_POINT ( 'NONE', #996 ) ;
#4464 = EDGE_LOOP ( 'NONE', ( #3106, #6620, #4993, #3953, #2784, #6167 ) ) ;
#4465 = CARTESIAN_POINT ( 'NONE',  ( 18.30767084474956263, 38.73487850452738002, 52.63397348499201200 ) ) ;
#4466 = LINE ( 'NONE', #2653, #5991 ) ;
#4467 = CARTESIAN_POINT ( 'NONE',  ( -0.3543307086614173040, 0.1379824317933223410, -0.3941213672119904809 ) ) ;
#4468 = CARTESIAN_POINT ( 'NONE',  ( 1.067758866085110281, 0.2211013871911202966, -0.9591012775692122627 ) ) ;
#4469 = DIRECTION ( 'NONE',  ( -1.000000000000000000, 0.000000000000000000, 0.000000000000000000 ) ) ;
#4470 = CARTESIAN_POINT ( 'NONE',  ( 0.3487102105009278197, -0.2024297391849458061, 0.2527898980517221394 ) ) ;
#4471 = FACE_OUTER_BOUND ( 'NONE', #5105, .T. ) ;
#4472 = CARTESIAN_POINT ( 'NONE',  ( -0.4416276115803083879, 1.010073413237866813, -1.570717210673253428 ) ) ;
#4473 = CARTESIAN_POINT ( 'NONE',  ( 0.4685039370078740717, -0.3409548833797009237, 0.000000000000000000 ) ) ;
#4474 = VERTEX_POINT ( 'NONE', #5133 ) ;
#4475 = DIRECTION ( 'NONE',  ( 0.000000000000000000, -1.224646799147353700E-16, 1.000000000000000000 ) ) ;
#4476 = CARTESIAN_POINT ( 'NONE',  ( 0.3528850351813199726, -0.3340780101605776986, -0.02497973507596915055 ) ) ;
#4477 = CARTESIAN_POINT ( 'NONE',  ( -0.9990286922241452539, -0.4596433552321293470, -1.415369843883348411 ) ) ;
#4478 = VERTEX_POINT ( 'NONE', #2821 ) ;
#4479 = CARTESIAN_POINT ( 'NONE',  ( 0.3321022367507226458, 0.2411754471855206694, -0.1728230530388957520 ) ) ;
#4480 = CARTESIAN_POINT ( 'NONE',  ( -0.9857970000181568437, -0.4541662050560865138, -1.560880783937514726 ) ) ;
#4481 = DIRECTION ( 'NONE',  ( 0.000000000000000000, 1.000000000000000000, 0.000000000000000000 ) ) ;
#4482 = ORIENTED_EDGE ( 'NONE', *, *, #6355, .T. ) ;
#4483 = ORIENTED_EDGE ( 'NONE', *, *, #1153, .T. ) ;
#4484 = CARTESIAN_POINT ( 'NONE',  ( 0.000000000000000000, 0.2557161625347750267, 0.1476377952755908163 ) ) ;
#4485 = CARTESIAN_POINT ( 'NONE',  ( 0.3528971332113846615, 0.1886393090946605622, 0.2768874834731247514 ) ) ;
#4486 = ADVANCED_FACE ( 'NONE', ( #1675 ), #5745, .T. ) ;
#4487 = CARTESIAN_POINT ( 'NONE',  ( 0.3483227611829848303, -0.1704774416898505729, -0.2952755905511810774 ) ) ;
#4488 = VERTEX_POINT ( 'NONE', #6771 ) ;
#4489 = CARTESIAN_POINT ( 'NONE',  ( 0.02637295201093697167, 0.1704774416898497680, -0.2952755905511810774 ) ) ;
#4490 = ORIENTED_EDGE ( 'NONE', *, *, #7513, .T. ) ;
#4491 = CARTESIAN_POINT ( 'NONE',  ( 0.4685039370078740717, 0.000000000000000000, 0.000000000000000000 ) ) ;
#4492 = ORIENTED_EDGE ( 'NONE', *, *, #6696, .F. ) ;
#4493 = DIRECTION ( 'NONE',  ( -3.491481338843133750E-15, 1.000000000000000000, 0.000000000000000000 ) ) ;
#4494 = ORIENTED_EDGE ( 'NONE', *, *, #6125, .T. ) ;
#4495 = FACE_OUTER_BOUND ( 'NONE', #3281, .T. ) ;
#4496 = EDGE_CURVE ( 'NONE', #4488, #2144, #1427, .T. ) ;
#4497 = EDGE_CURVE ( 'NONE', #3371, #2290, #3766, .T. ) ;
#4498 = DIRECTION ( 'NONE',  ( -1.000000000000000000, -6.436324498194463255E-16, -2.251170071535830774E-15 ) ) ;
#4499 = CIRCLE ( 'NONE', #1171, 1.223643328182681289 ) ;
#4500 = DIRECTION ( 'NONE',  ( 1.224646799147353207E-16, 1.000000000000000000, 0.000000000000000000 ) ) ;
#4501 = FACE_OUTER_BOUND ( 'NONE', #1485, .T. ) ;
#4502 = SURFACE_STYLE_FILL_AREA ( #5222 ) ;
#4503 = CARTESIAN_POINT ( 'NONE',  ( 1.641312181851266274E-15, -0.4700904924197871204, -2.204724409448822975 ) ) ;
#4504 = B_SPLINE_CURVE_WITH_KNOTS ( 'NONE', 3,
 ( #1649, #7380, #5604, #2190, #2796, #2151, #7342, #6854, #4485, #3956 ),
 .UNSPECIFIED., .F., .F.,
 ( 4, 2, 2, 2, 4 ),
 ( 0.000000000000000000, 0.002239656411828510555, 0.004479312823657022845, 0.006718969235485534701, 0.008958625647314047424 ),
 .UNSPECIFIED. ) ;
#4505 = DIRECTION ( 'NONE',  ( -1.000000000000000000, 0.000000000000000000, 0.000000000000000000 ) ) ;
#4506 = AXIS2_PLACEMENT_3D ( 'NONE', #6208, #70, #5721 ) ;
#4507 = CARTESIAN_POINT ( 'NONE',  ( 0.3496779274129794279, -0.3447056852546012129, -0.006496579416451788574 ) ) ;
#4508 = CARTESIAN_POINT ( 'NONE',  ( 0.003035684155427131534, 0.2845908893795032757, 0.09762530132584859577 ) ) ;
#4509 = ORIENTED_EDGE ( 'NONE', *, *, #2620, .T. ) ;
#4510 = CARTESIAN_POINT ( 'NONE',  ( 0.02637295201093707228, -0.1704774416898499345, 0.2952755905511811330 ) ) ;
#4511 = EDGE_LOOP ( 'NONE', ( #2523, #2868, #404, #884 ) ) ;
#4512 = CIRCLE ( 'NONE', #3408, 0.3543307086614173596 ) ;
#4513 = CARTESIAN_POINT ( 'NONE',  ( 0.3432736861146659657, 0.1420645347415416815, 0.2952755905511811330 ) ) ;
#4514 = CARTESIAN_POINT ( 'NONE',  ( 0.2371803407075526726, 0.2722097265016474310, -0.4046248963849245484 ) ) ;
#4515 = DIRECTION ( 'NONE',  ( 0.000000000000000000, 0.000000000000000000, -1.000000000000000000 ) ) ;
#4516 = DIRECTION ( 'NONE',  ( 4.647695938698652561E-15, 1.421085471520200372E-14, -1.000000000000000000 ) ) ;
#4517 = ORIENTED_EDGE ( 'NONE', *, *, #99, .F. ) ;
#4518 = CARTESIAN_POINT ( 'NONE',  ( 0.3565422270302655572, 0.1673297761639317704, -0.3007275071673040645 ) ) ;
#4519 = CARTESIAN_POINT ( 'NONE',  ( 0.3442723180357430413, -0.1814473180894617399, 0.2762752072743029363 ) ) ;
#4520 = ORIENTED_EDGE ( 'NONE', *, *, #5374, .F. ) ;
#4521 = ORIENTED_EDGE ( 'NONE', *, *, #1877, .T. ) ;
#4522 = AXIS2_PLACEMENT_3D ( 'NONE', #4415, #3563, #1671 ) ;
#4523 = CARTESIAN_POINT ( 'NONE',  ( -0.4353079511162236681, 0.9479499796399324385, -1.456692913385828625 ) ) ;
#4524 = SURFACE_STYLE_USAGE ( .BOTH. , #6245 ) ;
#4525 = ORIENTED_EDGE ( 'NONE', *, *, #4462, .F. ) ;
#4526 = FACE_BOUND ( 'NONE', #6675, .T. ) ;
#4527 = VERTEX_POINT ( 'NONE', #1641 ) ;
#4528 = CARTESIAN_POINT ( 'NONE',  ( 0.3585665126877356501, 0.3496831043983829046, -0.001800812819183686539 ) ) ;
#4529 = ADVANCED_FACE ( 'NONE', ( #2221 ), #6818, .T. ) ;
#4530 = ORIENTED_EDGE ( 'NONE', *, *, #488, .T. ) ;
#4531 = DIRECTION ( 'NONE',  ( 0.000000000000000000, 0.000000000000000000, 1.000000000000000000 ) ) ;
#4532 = DIRECTION ( 'NONE',  ( 0.9991895563372416023, -0.04025208698423499848, 8.530088470648690983E-16 ) ) ;
#4533 = MECHANICAL_DESIGN_GEOMETRIC_PRESENTATION_REPRESENTATION (  '', ( #6851 ), #5028 ) ;
#4534 = DIRECTION ( 'NONE',  ( 0.000000000000000000, 0.000000000000000000, -1.000000000000000000 ) ) ;
#4535 =( NAMED_UNIT ( * ) PLANE_ANGLE_UNIT ( ) SI_UNIT ( $, .RADIAN. ) );
#4536 = CARTESIAN_POINT ( 'NONE',  ( -5.972582710757682675E-17, -0.2484822268960368286, 0.1601673393405688428 ) ) ;
#4537 = CARTESIAN_POINT ( 'NONE',  ( 1.060506290833840293, 0.2237082381425291866, -0.9584946220175588616 ) ) ;
#4538 = EDGE_CURVE ( 'NONE', #7001, #3252, #3179, .T. ) ;
#4539 = EDGE_CURVE ( 'NONE', #7188, #139, #1934, .T. ) ;
#4540 = CIRCLE ( 'NONE', #386, 0.2362204724409449896 ) ;
#4541 = EDGE_CURVE ( 'NONE', #2119, #2829, #590, .T. ) ;
#4542 = DIRECTION ( 'NONE',  ( -1.000000000000000000, -0.000000000000000000, -0.000000000000000000 ) ) ;
#4543 = CARTESIAN_POINT ( 'NONE',  ( 0.3585665126877354281, -0.1732820025503174766, 0.3037348580927970443 ) ) ;
#4544 = CARTESIAN_POINT ( 'NONE',  ( 0.000000000000000000, 0.000000000000000000, 0.000000000000000000 ) ) ;
#4545 = AXIS2_PLACEMENT_3D ( 'NONE', #3448, #479, #5819 ) ;
#4546 = DIRECTION ( 'NONE',  ( 0.000000000000000000, -0.8660254037844379305, 0.5000000000000013323 ) ) ;
#4547 = ADVANCED_FACE ( 'NONE', ( #6380 ), #68, .F. ) ;
#4548 = ORIENTED_EDGE ( 'NONE', *, *, #6355, .F. ) ;
#4549 = CIRCLE ( 'NONE', #1232, 1.968503937007874072 ) ;
#4550 = DIRECTION ( 'NONE',  ( -1.000000000000000000, 0.000000000000000000, 0.000000000000000000 ) ) ;
#4551 = B_SPLINE_CURVE_WITH_KNOTS ( 'NONE', 3,
 ( #5056, #3286, #959, #4443, #3365, #7333, #1062, #433 ),
 .UNSPECIFIED., .F., .F.,
 ( 4, 2, 2, 4 ),
 ( 0.005257893453559899302, 0.006567392922673231243, 0.007876892391786563183, 0.01049589133001322706 ),
 .UNSPECIFIED. ) ;
#4552 = DIRECTION ( 'NONE',  ( 0.000000000000000000, 0.000000000000000000, 1.000000000000000000 ) ) ;
#4553 = ITEM_DEFINED_TRANSFORMATION ( 'NONE', 'NONE', #527,  #5166 ) ;
#4554 = CARTESIAN_POINT ( 'NONE',  ( -0.9696655408443565216, -0.5073440712898458216, -1.367310953805257023 ) ) ;
#4555 = EDGE_LOOP ( 'NONE', ( #3151, #7013, #2014, #1779 ) ) ;
#4556 = AXIS2_PLACEMENT_3D ( 'NONE', #914, #6689, #7256 ) ;
#4557 = CARTESIAN_POINT ( 'NONE',  ( 6.500080172145040803E-30, -1.861696953619914682E-15, -1.361499588670820771 ) ) ;
#4558 = CARTESIAN_POINT ( 'NONE',  ( 0.000000000000000000, 0.000000000000000000, 0.000000000000000000 ) ) ;
#4559 = EDGE_LOOP ( 'NONE', ( #5574, #6712 ) ) ;
#4560 = ORIENTED_EDGE ( 'NONE', *, *, #1154, .F. ) ;
#4561 = CIRCLE ( 'NONE', #877, 0.2362204724409449619 ) ;
#4562 = CARTESIAN_POINT ( 'NONE',  ( -0.3253487914207032206, 0.2213056477483777151, -0.02198690333287076776 ) ) ;
#4563 = CARTESIAN_POINT ( 'NONE',  ( 0.3391892065151629332, -0.1136516277932338725, -0.2952755905511810774 ) ) ;
#4564 = EDGE_LOOP ( 'NONE', ( #232, #5758, #6881, #4853, #3654, #3410, #924 ) ) ;
#4565 = CARTESIAN_POINT ( 'NONE',  ( 0.01834252172841625839, 0.1843865549457985864, -0.2711842997036481573 ) ) ;
#4566 = ORIENTED_EDGE ( 'NONE', *, *, #4674, .T. ) ;
#4567 = CARTESIAN_POINT ( 'NONE',  ( -0.2962704110120346623, -0.2380940585049214631, -0.3942118233966396268 ) ) ;
#4568 = B_SPLINE_CURVE_WITH_KNOTS ( 'NONE', 3,
 ( #5551, #2063, #6721, #3625, #3277, #422, #4583, #5589 ),
 .UNSPECIFIED., .F., .F.,
 ( 4, 2, 2, 4 ),
 ( -7.690028535486727074E-06, 0.001102852776893269420, 0.001658124179607644048, 0.002213395582322019110 ),
 .UNSPECIFIED. ) ;
#4569 = PLANE ( 'NONE',  #5141 ) ;
#4570 = VERTEX_POINT ( 'NONE', #3546 ) ;
#4571 = DIRECTION ( 'NONE',  ( -0.000000000000000000, -1.000000000000000000, -0.000000000000000000 ) ) ;
#4572 = DIRECTION ( 'NONE',  ( -1.000000000000000000, -8.648785545355717899E-18, -2.320548612096681119E-16 ) ) ;
#4573 = PRODUCT_RELATED_PRODUCT_CATEGORY ( 'part', '', ( #1216 ) ) ;
#4574 = DIRECTION ( 'NONE',  ( 0.000000000000000000, 0.000000000000000000, 1.000000000000000000 ) ) ;
#4575 =( CONVERSION_BASED_UNIT ( 'INCH', #4641 ) LENGTH_UNIT ( ) NAMED_UNIT ( #436 ) );
#4576 = AXIS2_PLACEMENT_3D ( 'NONE', #3363, #4586, #7406 ) ;
#4577 = CARTESIAN_POINT ( 'NONE',  ( 0.003035684155427232581, -0.2268414356900468332, 0.1976502892253331478 ) ) ;
#4578 = DIRECTION ( 'NONE',  ( -1.000000000000000000, -0.000000000000000000, -0.000000000000000000 ) ) ;
#4579 = LENGTH_MEASURE_WITH_UNIT ( LENGTH_MEASURE( 0.02539999999999999897 ), #458 );
#4580 =( REPRESENTATION_RELATIONSHIP ('NONE','NONE', #303, #5265 ) REPRESENTATION_RELATIONSHIP_WITH_TRANSFORMATION ( #1820 )SHAPE_REPRESENTATION_RELATIONSHIP( ) );
#4581 = EDGE_CURVE ( 'NONE', #4777, #6862, #3476, .T. ) ;
#4582 = CARTESIAN_POINT ( 'NONE',  ( 0.3527006543068525457, -0.1709223289430796822, -0.2960461578774135627 ) ) ;
#4583 = CARTESIAN_POINT ( 'NONE',  ( 1.030265823844203288, -0.4349482548737160781, -1.574803149606299524 ) ) ;
#4584 = UNCERTAINTY_MEASURE_WITH_UNIT (LENGTH_MEASURE( 1.000000000000000082E-05 ), #6521, 'distance_accuracy_value', 'NONE');
#4585 = FACE_OUTER_BOUND ( 'NONE', #4103, .T. ) ;
#4586 = DIRECTION ( 'NONE',  ( 1.000000000000000000, 0.000000000000000000, 0.000000000000000000 ) ) ;
#4587 = CARTESIAN_POINT ( 'NONE',  ( 1.968503937007874072, 1.496062992125984259, -0.4921259842519685179 ) ) ;
#4588 = EDGE_CURVE ( 'NONE', #4449, #1388, #6284, .T. ) ;
#4589 = DIRECTION ( 'NONE',  ( -1.000000000000000000, -3.552713678800500929E-15, 0.000000000000000000 ) ) ;
#4590 = EDGE_CURVE ( 'NONE', #6581, #2461, #715, .T. ) ;
#4591 = DIRECTION ( 'NONE',  ( -1.000000000000000000, -0.000000000000000000, -4.625929269271482167E-15 ) ) ;
#4592 = VERTEX_POINT ( 'NONE', #4159 ) ;
#4593 = CARTESIAN_POINT ( 'NONE',  ( 1.070856907295309801, -0.4375700573520588943, -1.565644078513316106 ) ) ;
#4594 = CARTESIAN_POINT ( 'NONE',  ( 0.3531511627980760681, 0.1878266560944092389, -0.2783075040405467715 ) ) ;
#4595 = ADVANCED_FACE ( 'NONE', ( #1741 ), #351, .T. ) ;
#4596 = B_SPLINE_CURVE_WITH_KNOTS ( 'NONE', 3,
 ( #5253, #6559, #3605, #4221, #5830, #2454 ),
 .UNSPECIFIED., .F., .F.,
 ( 4, 2, 4 ),
 ( 2.380730968297687428E-07, 0.002629065763328357428, 0.005257893453559884557 ),
 .UNSPECIFIED. ) ;
#4597 = ORIENTED_EDGE ( 'NONE', *, *, #5542, .T. ) ;
#4598 = CARTESIAN_POINT ( 'NONE',  ( 0.9531588649300888338, -0.2346757028646479781, 0.9558707923556580832 ) ) ;
#4599 = FACE_OUTER_BOUND ( 'NONE', #7388, .T. ) ;
#4600 = CARTESIAN_POINT ( 'NONE',  ( 0.004822332172886080806, 0.2197023059474403073, -0.2100156246613533173 ) ) ;
#4601 = VERTEX_POINT ( 'NONE', #33 ) ;
#4602 = DIRECTION ( 'NONE',  ( -1.000000000000000000, 0.000000000000000000, 0.000000000000000000 ) ) ;
#4603 = CARTESIAN_POINT ( 'NONE',  ( -0.9659644734970558311, 0.4700904924197872314, -1.546597720061112069 ) ) ;
#4604 = ORIENTED_EDGE ( 'NONE', *, *, #5904, .F. ) ;
#4605 = LINE ( 'NONE', #5252, #1608 ) ;
#4606 = DIRECTION ( 'NONE',  ( 0.000000000000000000, 0.000000000000000000, 1.000000000000000000 ) ) ;
#4607 = CARTESIAN_POINT ( 'NONE',  ( 0.9159932075028710541, 0.4466261709646471290, -1.451746187131335519 ) ) ;
#4608 = DIRECTION ( 'NONE',  ( -0.000000000000000000, 0.000000000000000000, -1.000000000000000000 ) ) ;
#4609 = CARTESIAN_POINT ( 'NONE',  ( -1.003669596044583168, -0.4445636273010842854, -1.568530023225017223 ) ) ;
#4610 = AXIS2_PLACEMENT_3D ( 'NONE', #6285, #2727, #2833 ) ;
#4611 = CARTESIAN_POINT ( 'NONE',  ( -0.5118110236220474452, 1.220472440944881942, 0.4724409448818898127 ) ) ;
#4612 = FACE_OUTER_BOUND ( 'NONE', #297, .T. ) ;
#4613 = AXIS2_PLACEMENT_3D ( 'NONE', #2859, #1280, #542 ) ;
#4614 = DIRECTION ( 'NONE',  ( -1.000000000000000000, 0.000000000000000000, 0.000000000000000000 ) ) ;
#4615 = EDGE_CURVE ( 'NONE', #5146, #6892, #3272, .T. ) ;
#4616 = CARTESIAN_POINT ( 'NONE',  ( -0.8785537298370134085, 0.4700904924197875645, -1.433776001880362250 ) ) ;
#4617 = CARTESIAN_POINT ( 'NONE',  ( 0.3585664987351884214, -0.1764010263750315499, -0.3019340449705225082 ) ) ;
#4618 = CIRCLE ( 'NONE', #6942, 1.278433327952054999 ) ;
#4619 = DIRECTION ( 'NONE',  ( 0.000000000000000000, 0.000000000000000000, 1.000000000000000000 ) ) ;
#4620 = EDGE_LOOP ( 'NONE', ( #5185, #2424, #6394, #5371, #3683 ) ) ;
#4622 = DIRECTION ( 'NONE',  ( -0.000000000000000000, -0.000000000000000000, 1.000000000000000000 ) ) ;
#4621 = DIMENSIONAL_EXPONENTS ( 1.000000000000000000, 0.000000000000000000, 0.000000000000000000, 0.000000000000000000, 0.000000000000000000, 0.000000000000000000, 0.000000000000000000 ) ;
#4623 = CARTESIAN_POINT ( 'NONE',  ( 0.3496779274129794279, -0.3447056852546012129, -0.006496579416451788574 ) ) ;
#4624 = CIRCLE ( 'NONE', #1436, 0.2362204724409449341 ) ;
#4625 = EDGE_CURVE ( 'NONE', #4753, #6362, #1682, .T. ) ;
#4626 = ADVANCED_FACE ( 'NONE', ( #6499 ), #111, .F. ) ;
#4627 = ORIENTED_EDGE ( 'NONE', *, *, #4017, .F. ) ;
#4628 = ORIENTED_EDGE ( 'NONE', *, *, #1441, .T. ) ;
#4629 = LINE ( 'NONE', #6351, #2101 ) ;
#4630 = ADVANCED_FACE ( 'NONE', ( #685 ), #5609, .T. ) ;
#4631 = CARTESIAN_POINT ( 'NONE',  ( 0.3485373078438441796, 0.2031105961982143382, -0.2516016230262507203 ) ) ;
#4632 = ORIENTED_EDGE ( 'NONE', *, *, #6678, .F. ) ;
#4633 = FACE_OUTER_BOUND ( 'NONE', #2803, .T. ) ;
#4634 = CYLINDRICAL_SURFACE ( 'NONE', #118, 0.2362204724409448231 ) ;
#4635 = ADVANCED_FACE ( 'NONE', ( #4200 ), #6538, .F. ) ;
#4636 = VERTEX_POINT ( 'NONE', #5470 ) ;
#4637 = AXIS2_PLACEMENT_3D ( 'NONE', #7356, #5545, #1977 ) ;
#4638 = CARTESIAN_POINT ( 'NONE',  ( 0.9842519685039370358, 1.220472440944881942, 2.480314960629921295 ) ) ;
#4639 =( LENGTH_UNIT ( ) NAMED_UNIT ( * ) SI_UNIT ( $, .METRE. ) );
#4640 = CARTESIAN_POINT ( 'NONE',  ( 0.9044351468059328436, 0.4526810454163415209, -1.447629383090424993 ) ) ;
#4641 = LENGTH_MEASURE_WITH_UNIT ( LENGTH_MEASURE( 0.02539999999999999897 ), #455 );
#4642 = CARTESIAN_POINT ( 'NONE',  ( -1.056523642887401415, -0.5141614760841493048, -1.484898342931014303 ) ) ;
#4643 = CARTESIAN_POINT ( 'NONE',  ( -0.4338950423154138147, 1.037563309807725043, -1.574803149606299302 ) ) ;
#4644 = TOROIDAL_SURFACE ( 'NONE', #1967, 1.223643328182681289, 0.05905511811023622659 ) ;
#4645 = CARTESIAN_POINT ( 'NONE',  ( 0.2362204724409449619, 0.000000000000000000, -0.4082677165354330340 ) ) ;
#4646 = CARTESIAN_POINT ( 'NONE',  ( 0.7480314960629922405, 1.220472440944881942, 2.952755905511811108 ) ) ;
#4647 = AXIS2_PLACEMENT_3D ( 'NONE', #4925, #2058, #1982 ) ;
#4648 = CARTESIAN_POINT ( 'NONE',  ( 0.3321025531238107620, -0.02909241602403181068, -0.2952755905511810774 ) ) ;
#4649 = DIRECTION ( 'NONE',  ( 0.000000000000000000, 0.000000000000000000, 1.000000000000000000 ) ) ;
#4650 = CARTESIAN_POINT ( 'NONE',  ( 0.3543307086614172485, 0.000000000000000000, 0.1188976377952756375 ) ) ;
#4651 = AXIS2_PLACEMENT_3D ( 'NONE', #3347, #2090, #333 ) ;
#4652 = CONTEXT_DEPENDENT_SHAPE_REPRESENTATION ( #2770, #6072 ) ;
#4653 = CARTESIAN_POINT ( 'NONE',  ( -0.4514963146295076224, -0.9983958463931812410, -1.424958914991361292 ) ) ;
#4654 = VERTEX_POINT ( 'NONE', #1907 ) ;
#4655 = LINE ( 'NONE', #4735, #6382 ) ;
#4656 = CARTESIAN_POINT ( 'NONE',  ( 0.3581828924050327045, -0.3486337532542230222, -1.123169198254405176E-18 ) ) ;
#4657 = AXIS2_PLACEMENT_3D ( 'NONE', #6295, #3384, #1500 ) ;
#4658 = ORIENTED_EDGE ( 'NONE', *, *, #3271, .F. ) ;
#4659 = EDGE_LOOP ( 'NONE', ( #3531, #608, #5023, #6094 ) ) ;
#4660 = CARTESIAN_POINT ( 'NONE',  ( 0.000000000000000000, 0.000000000000000000, 0.000000000000000000 ) ) ;
#4661 = CIRCLE ( 'NONE', #885, 0.2362204724409449064 ) ;
#4662 = EDGE_CURVE ( 'NONE', #4592, #4449, #1813, .T. ) ;
#4663 = DIRECTION ( 'NONE',  ( -1.000000000000000000, -0.000000000000000000, -0.000000000000000000 ) ) ;
#4664 = EDGE_CURVE ( 'NONE', #6137, #4020, #5030, .T. ) ;
#4665 = ORIENTED_EDGE ( 'NONE', *, *, #1471, .T. ) ;
#4666 = CARTESIAN_POINT ( 'NONE',  ( 0.3485616995351332181, -0.1165012447190267864, -0.3017003685801735724 ) ) ;
#4667 = CYLINDRICAL_SURFACE ( 'NONE', #2198, 0.2362204724409448231 ) ;
#4668 = DIRECTION ( 'NONE',  ( 1.000000000000000000, 0.000000000000000000, -0.000000000000000000 ) ) ;
#4669 = EDGE_CURVE ( 'NONE', #5183, #1296, #2895, .T. ) ;
#4670 = ORIENTED_EDGE ( 'NONE', *, *, #2568, .T. ) ;
#4671 = VECTOR ( 'NONE', #5475, 39.37007874015748143 ) ;
#4672 = CARTESIAN_POINT ( 'NONE',  ( 0.000000000000000000, 0.000000000000000000, 0.1783464566929134354 ) ) ;
#4673 = DIRECTION ( 'NONE',  ( -1.000000000000000000, 3.552713678800500929E-15, 0.000000000000000000 ) ) ;
#4674 = EDGE_CURVE ( 'NONE', #3477, #4341, #2057, .T. ) ;
#4675 = CARTESIAN_POINT ( 'NONE',  ( -0.4921259842519648542, 0.000000000000000000, -2.204724409448822975 ) ) ;
#4676 = EDGE_CURVE ( 'NONE', #2077, #2074, #5675, .T. ) ;
#4677 = CARTESIAN_POINT ( 'NONE',  ( -0.4330708661417320138, -0.9604263920613191896, -1.456063616177416087 ) ) ;
#4678 = CARTESIAN_POINT ( 'NONE',  ( -1.080458485393810397, -0.4837908950006702402, -1.514208454829283346 ) ) ;
#4679 = AXIS2_PLACEMENT_3D ( 'NONE', #1735, #2309, #1090 ) ;
#4680 = DIRECTION ( 'NONE',  ( -1.000000000000000000, 0.000000000000000000, 0.000000000000000000 ) ) ;
#4681 = ORIENTED_EDGE ( 'NONE', *, *, #900, .F. ) ;
#4682 = CLOSED_SHELL ( 'NONE', ( #4626, #6343, #2765, #7471, #6360, #5631, #660, #1400, #1067, #6041, #3841, #7374, #3734, #2723, #5628, #7010, #234, #4208, #7048, #4823, #7470, #3191 ) ) ;
#4683 = CARTESIAN_POINT ( 'NONE',  ( 0.3585665126877357611, -0.3496831043983833487, 0.001800812819183493984 ) ) ;
#4684 = CARTESIAN_POINT ( 'NONE',  ( 0.3581828924050324825, -0.1743168766271116221, -0.3019256869348722061 ) ) ;
#4685 = DIRECTION ( 'NONE',  ( 1.000000000000000000, 0.000000000000000000, 0.000000000000000000 ) ) ;
#4686 = CARTESIAN_POINT ( 'NONE',  ( 0.7480314960629922405, 1.220472440944881942, 0.4724409448818898127 ) ) ;
#4687 = AXIS2_PLACEMENT_3D ( 'NONE', #1048, #410, #791 ) ;
#4688 =( GEOMETRIC_REPRESENTATION_CONTEXT ( 3 ) GLOBAL_UNCERTAINTY_ASSIGNED_CONTEXT ( ( #464 ) ) GLOBAL_UNIT_ASSIGNED_CONTEXT ( ( #7315, #2018, #2055 ) ) REPRESENTATION_CONTEXT ( 'NONE', 'WORKASPACE' ) );
#4689 = CARTESIAN_POINT ( 'NONE',  ( 0.9666437042230172638, -0.4330708661417221883, -1.454455828411335583 ) ) ;
#4690 = CARTESIAN_POINT ( 'NONE',  ( 1.512058847530478993E-15, -0.4330708661417287941, -2.204724409448822975 ) ) ;
#4691 = CARTESIAN_POINT ( 'NONE',  ( 0.3391892065151629332, 0.3125419764313920323, 0.04921259842519686012 ) ) ;
#4692 = CARTESIAN_POINT ( 'NONE',  ( 0.3528999085283635040, 0.1454870853231265693, 0.3018102362147644380 ) ) ;
#4693 = EDGE_LOOP ( 'NONE', ( #6248, #895, #3011, #2086, #3594, #1181, #4597, #3874, #3595, #1026, #4509 ) ) ;
#4694 = FACE_OUTER_BOUND ( 'NONE', #1335, .T. ) ;
#4695 = DIRECTION ( 'NONE',  ( 0.000000000000000000, -0.000000000000000000, 1.000000000000000000 ) ) ;
#4696 = VERTEX_POINT ( 'NONE', #2026 ) ;
#4697 = VERTEX_POINT ( 'NONE', #7253 ) ;
#4698 = CARTESIAN_POINT ( 'NONE',  ( 0.8465112843344620996, -0.1920587529112295633, 0.9653415754825105388 ) ) ;
#4699 = LINE ( 'NONE', #5403, #90 ) ;
#4700 = ORIENTED_EDGE ( 'NONE', *, *, #4676, .F. ) ;
#4701 = CARTESIAN_POINT ( 'NONE',  ( 0.4685039370078740717, 0.1704774416898499345, 0.2952755905511810774 ) ) ;
#4702 = CARTESIAN_POINT ( 'NONE',  ( -1.037563309807726375, 0.4338950423154108171, -1.574803149606299302 ) ) ;
#4703 = VERTEX_POINT ( 'NONE', #192 ) ;
#4704 = EDGE_CURVE ( 'NONE', #4133, #7450, #3395, .T. ) ;
#4705 = DIRECTION ( 'NONE',  ( -0.000000000000000000, -0.000000000000000000, 1.000000000000000000 ) ) ;
#4706 = CARTESIAN_POINT ( 'NONE',  ( 0.3531509790457915132, 0.1471070558423459573, 0.3018164037399326816 ) ) ;
#4707 = APPLICATION_PROTOCOL_DEFINITION ( 'draft international standard', 'automotive_design', 1998, #2474 ) ;
#4708 = UNCERTAINTY_MEASURE_WITH_UNIT (LENGTH_MEASURE( 1.000000000000000082E-05 ), #3228, 'distance_accuracy_value', 'NONE');
#4709 = CARTESIAN_POINT ( 'NONE',  ( 8.136851934253910637E-18, -0.02882762270234999827, 0.2952755905511811330 ) ) ;
#4710 = DIRECTION ( 'NONE',  ( 0.000000000000000000, 0.000000000000000000, -1.000000000000000000 ) ) ;
#4711 = DIRECTION ( 'NONE',  ( 0.000000000000000000, 0.000000000000000000, 1.000000000000000000 ) ) ;
#4712 = AXIS2_PLACEMENT_3D ( 'NONE', #2908, #2305, #5191 ) ;
#4713 = FACE_OUTER_BOUND ( 'NONE', #5449, .T. ) ;
#4714 = CARTESIAN_POINT ( 'NONE',  ( -0.9659644734970528335, -0.4700904924197936707, -1.546597720061111847 ) ) ;
#4715 =( REPRESENTATION_RELATIONSHIP ('NONE','NONE', #303, #7075 ) REPRESENTATION_RELATIONSHIP_WITH_TRANSFORMATION ( #5780 )SHAPE_REPRESENTATION_RELATIONSHIP( ) );
#4716 = EDGE_CURVE ( 'NONE', #7498, #2124, #7051, .T. ) ;
#4717 = ORIENTED_EDGE ( 'NONE', *, *, #7147, .T. ) ;
#4718 = EDGE_CURVE ( 'NONE', #929, #1000, #4391, .T. ) ;
#4719 = CARTESIAN_POINT ( 'NONE',  ( 0.3442723180356911383, -0.3299850069800938646, -0.01900038327687023423 ) ) ;
#4720 = CYLINDRICAL_SURFACE ( 'NONE', #5634, 0.2362204724409449064 ) ;
#4721 = FACE_OUTER_BOUND ( 'NONE', #1783, .T. ) ;
#4722 = DIRECTION ( 'NONE',  ( -0.000000000000000000, -0.000000000000000000, -1.000000000000000000 ) ) ;
#4723 = CARTESIAN_POINT ( 'NONE',  ( 0.3487105584742864473, -0.1177098269287414900, -0.3017042544367490309 ) ) ;
#4724 = AXIS2_PLACEMENT_3D ( 'NONE', #3636, #1291, #2366 ) ;
#4725 = CARTESIAN_POINT ( 'NONE',  ( 0.3483227611829846637, 0.1704774416898499345, 0.2952755905511810774 ) ) ;
#4726 =( BOUNDED_SURFACE ( )  B_SPLINE_SURFACE ( 3, 2, ( 
 ( #1475, #5558, #6162 ),
 ( #917, #846, #5483 ),
 ( #317, #3245, #239 ),
 ( #2634, #4975, #5595 ),
 ( #2671, #1371, #5443 ),
 ( #3717, #202, #2524 ),
 ( #4854, #1951, #6058 ),
 ( #1060, #3398, #4617 ) ),
 .UNSPECIFIED., .F., .F., .F. ) 
 B_SPLINE_SURFACE_WITH_KNOTS ( ( 4, 2, 2, 4 ),
 ( 3, 3 ),
 ( 0.03552366018096265315, 0.03995354946645690575, 0.04216849410920403551, 0.04438343875195116528 ),
 ( 0.000000000000000000, 1.000000000000000000 ),
 .UNSPECIFIED. ) 
 GEOMETRIC_REPRESENTATION_ITEM ( )  RATIONAL_B_SPLINE_SURFACE ( (
 ( 1.000000000000000000, 0.8047780977832075244, 1.000000000000000000),
 ( 1.000000000000000000, 0.8123789484488428414, 1.000000000000000000),
 ( 1.000000000000000000, 0.8190677874188468932, 1.000000000000000000),
 ( 1.000000000000000000, 0.8191929099079664489, 1.000000000000000000),
 ( 1.000000000000000000, 0.8176081235728045460, 1.000000000000000000),
 ( 1.000000000000000000, 0.8122952617572927192, 1.000000000000000000),
 ( 1.000000000000000000, 0.8086306736854887989, 1.000000000000000000),
 ( 1.000000000000000000, 0.8047712637616463160, 1.000000000000000000) ) ) 
 REPRESENTATION_ITEM ( '' )  SURFACE ( )  );
#4727 = CARTESIAN_POINT ( 'NONE',  ( -0.4762527114670029316, 0.9941396836775485690, -1.397361282224858892 ) ) ;
#4728 = CARTESIAN_POINT ( 'NONE',  ( 0.3306743754077733355, 0.2557161625347751932, 0.1476377952755905942 ) ) ;
#4729 = DIRECTION ( 'NONE',  ( -1.000000000000000000, -0.000000000000000000, -0.000000000000000000 ) ) ;
#4730 = AXIS2_PLACEMENT_3D ( 'NONE', #5485, #5446, #3098 ) ;
#4731 = DIRECTION ( 'NONE',  ( 1.000000000000000000, 0.000000000000000000, 0.000000000000000000 ) ) ;
#4732 = LINE ( 'NONE', #1823, #1941 ) ;
#4733 = CARTESIAN_POINT ( 'NONE',  ( 0.3483227611829848303, -0.1704774416898505729, -0.2952755905511810774 ) ) ;
#4734 = VERTEX_POINT ( 'NONE', #6081 ) ;
#4735 = CARTESIAN_POINT ( 'NONE',  ( 1.968503937007874072, 1.496062992125984259, -0.2362204724409449619 ) ) ;
#4736 = PLANE ( 'NONE',  #2316 ) ;
#4737 = ORIENTED_EDGE ( 'NONE', *, *, #427, .F. ) ;
#4738 = AXIS2_PLACEMENT_3D ( 'NONE', #6356, #1006, #1572 ) ;
#4739 = VERTEX_POINT ( 'NONE', #4846 ) ;
#4740 = CARTESIAN_POINT ( 'NONE',  ( 1.377952755905512028, 0.7480314960629921295, -0.7480314960629921295 ) ) ;
#4741 = DIRECTION ( 'NONE',  ( -1.000000000000000000, -3.516270216102430554E-15, 0.000000000000000000 ) ) ;
#4742 = EDGE_LOOP ( 'NONE', ( #674, #6253, #5214, #2038 ) ) ;
#4743 = AXIS2_PLACEMENT_3D ( 'NONE', #911, #982, #3276 ) ;
#4744 = CARTESIAN_POINT ( 'NONE',  ( 0.4514965799695757620, 0.9983959133492256166, -1.424958590981960871 ) ) ;
#4745 = ORIENTED_EDGE ( 'NONE', *, *, #49, .T. ) ;
#4746 = EDGE_LOOP ( 'NONE', ( #6418, #6963, #7126, #2497, #3549, #2756 ) ) ;
#4747 = DIRECTION ( 'NONE',  ( -0.000000000000000000, -0.000000000000000000, 1.000000000000000000 ) ) ;
#4748 = AXIS2_PLACEMENT_3D ( 'NONE', #1138, #1884, #7035 ) ;
#4749 = CARTESIAN_POINT ( 'NONE',  ( 0.3585665266928871331, 0.1764011776056260972, 0.3019340455778471433 ) ) ;
#4750 = DIRECTION ( 'NONE',  ( 0.000000000000000000, 0.000000000000000000, 1.000000000000000000 ) ) ;
#4751 = SURFACE_STYLE_USAGE ( .BOTH. , #2499 ) ;
#4752 = CARTESIAN_POINT ( 'NONE',  ( 0.3459468362671123676, -0.1200707489736706907, 0.2952755905511811885 ) ) ;
#4753 = VERTEX_POINT ( 'NONE', #4352 ) ;
#4754 = CARTESIAN_POINT ( 'NONE',  ( -1.070856827570678238, -0.4375700189966333364, -1.565644132322241644 ) ) ;
#4755 = ADVANCED_FACE ( 'NONE', ( #797 ), #5511, .T. ) ;
#4756 = ORIENTED_EDGE ( 'NONE', *, *, #1290, .T. ) ;
#4757 = B_SPLINE_CURVE_WITH_KNOTS ( 'NONE', 3,
 ( #5381, #3115, #2019, #222, #7133, #4923 ),
 .UNSPECIFIED., .F., .F.,
 ( 4, 2, 4 ),
 ( 0.004466737480205778058, 0.006712681563759909271, 0.008958625647314040485 ),
 .UNSPECIFIED. ) ;
#4758 = CARTESIAN_POINT ( 'NONE',  ( 0.2699662542182227343, 0.000000000000000000, 0.1783464566929134354 ) ) ;
#4759 = VERTEX_POINT ( 'NONE', #3204 ) ;
#4760 = CARTESIAN_POINT ( 'NONE',  ( 0.3585569128062319755, -0.1733077889112134284, -0.3036897776982950825 ) ) ;
#4761 = DIRECTION ( 'NONE',  ( -0.000000000000000000, -1.000000000000000000, -0.000000000000000000 ) ) ;
#4762 = ADVANCED_FACE ( 'NONE', ( #5392 ), #710, .T. ) ;
#4763 = DIRECTION ( 'NONE',  ( -1.000000000000000000, -0.000000000000000000, -0.000000000000000000 ) ) ;
#4764 = EDGE_CURVE ( 'NONE', #1492, #3685, #5391, .T. ) ;
#4765 = CARTESIAN_POINT ( 'NONE',  ( 0.3496779450092586949, 0.1779791412978203036, -0.2952755905511810774 ) ) ;
#4766 = EDGE_CURVE ( 'NONE', #781, #3685, #4568, .T. ) ;
#4767 = CARTESIAN_POINT ( 'NONE',  ( -1.279527559055118280, 1.968503937007874072, 2.952755905511811108 ) ) ;
#4768 = CARTESIAN_POINT ( 'NONE',  ( -0.4330708661417322913, 0.9666437042230143772, -1.454455828411337359 ) ) ;
#4769 = DIRECTION ( 'NONE',  ( 0.000000000000000000, 0.000000000000000000, 1.000000000000000000 ) ) ;
#4770 = CARTESIAN_POINT ( 'NONE',  ( 1.064252964791818634, 0.5072158114893481340, -1.491281854710859278 ) ) ;
#4771 = CIRCLE ( 'NONE', #7451, 0.2948818897637794922 ) ;
#4772 = CARTESIAN_POINT ( 'NONE',  ( 0.004822332172886149328, 0.2917300191221098293, 0.08525996588982816260 ) ) ;
#4773 = CARTESIAN_POINT ( 'NONE',  ( -0.7480314960629922405, 1.220472440944881942, 2.480314960629921295 ) ) ;
#4774 = FACE_OUTER_BOUND ( 'NONE', #4464, .T. ) ;
#4775 = DIRECTION ( 'NONE',  ( -0.8660254037844380415, -0.5000000000000007772, 0.000000000000000000 ) ) ;
#4776 = ADVANCED_FACE ( 'NONE', ( #504 ), #3975, .F. ) ;
#4777 = VERTEX_POINT ( 'NONE', #344 ) ;
#4778 = PRODUCT_DEFINITION_SHAPE ( 'NONE', 'NONE',  #5928 ) ;
#4779 = LINE ( 'NONE', #2890, #7117 ) ;
#4780 = CARTESIAN_POINT ( 'NONE',  ( 0.000000000000000000, 0.000000000000000000, 0.1188976377952756375 ) ) ;
#4781 = EDGE_LOOP ( 'NONE', ( #3746, #1098, #1403, #3515 ) ) ;
#4782 = CIRCLE ( 'NONE', #1464, 1.043121362164705745 ) ;
#4783 = CARTESIAN_POINT ( 'NONE',  ( 0.05806029764938262783, -0.3756247315785400387, -0.01405589313879368647 ) ) ;
#4784 = LINE ( 'NONE', #5900, #6934 ) ;
#4785 = AXIS2_PLACEMENT_3D ( 'NONE', #4503, #6835, #416 ) ;
#4786 = VERTEX_POINT ( 'NONE', #1549 ) ;
#4787 =( GEOMETRIC_REPRESENTATION_CONTEXT ( 3 ) GLOBAL_UNCERTAINTY_ASSIGNED_CONTEXT ( ( #1356 ) ) GLOBAL_UNIT_ASSIGNED_CONTEXT ( ( #1698, #3613, #2425 ) ) REPRESENTATION_CONTEXT ( 'NONE', 'WORKASPACE' ) );
#4788 = LINE ( 'NONE', #3560, #3817 ) ;
#4789 = VECTOR ( 'NONE', #11, 39.37007874015748143 ) ;
#4790 = DIRECTION ( 'NONE',  ( -0.000000000000000000, -0.000000000000000000, -1.000000000000000000 ) ) ;
#4791 = VERTEX_POINT ( 'NONE', #6761 ) ;
#4792 = EDGE_LOOP ( 'NONE', ( #5955, #5598, #1001, #5480 ) ) ;
#4793 = TOROIDAL_SURFACE ( 'NONE', #281, 1.124634398195722973, 0.05905511811023622659 ) ;
#4794 = DIRECTION ( 'NONE',  ( -0.000000000000000000, -1.000000000000000000, -0.000000000000000000 ) ) ;
#4795 = DIRECTION ( 'NONE',  ( 1.000000000000000000, 0.000000000000000000, -0.000000000000000000 ) ) ;
#4796 = FILL_AREA_STYLE_COLOUR ( '', #4035 ) ;
#4797 = DIRECTION ( 'NONE',  ( 1.000000000000000000, 0.000000000000000000, 0.000000000000000000 ) ) ;
#4798 = CARTESIAN_POINT ( 'NONE',  ( -1.078368813366568979, -0.4878045971890005994, -1.510181706589752038 ) ) ;
#4799 = ORIENTED_EDGE ( 'NONE', *, *, #3501, .F. ) ;
#4800 = AXIS2_PLACEMENT_3D ( 'NONE', #3206, #6160, #5514 ) ;
#4801 = CARTESIAN_POINT ( 'NONE',  ( 0.3425764178929368020, -0.2322094954269898481, 0.2008802154383053373 ) ) ;
#4802 = ORIENTED_EDGE ( 'NONE', *, *, #6913, .F. ) ;
#4803 = DIRECTION ( 'NONE',  ( 0.02486823048133330466, 0.6173114996811703836, -0.7863256853709609251 ) ) ;
#4804 = CONICAL_SURFACE ( 'NONE', #3576, 0.3543307086614173596, 1.047197551196596521 ) ;
#4805 = CARTESIAN_POINT ( 'NONE',  ( 0.3543307086614173040, 0.2045729300278205931, -0.03164754241312491001 ) ) ;
#4806 = CARTESIAN_POINT ( 'NONE',  ( 0.7480314960629922405, -0.01544581072159242723, -0.9842519685039369248 ) ) ;
#4807 = PLANE ( 'NONE',  #2956 ) ;
#4808 = CARTESIAN_POINT ( 'NONE',  ( 1.220472440944881942, 0.01566924555314537157, -0.9842519685039372579 ) ) ;
#4809 = UNCERTAINTY_MEASURE_WITH_UNIT (LENGTH_MEASURE( 1.000000000000000082E-05 ), #5297, 'distance_accuracy_value', 'NONE');
#4810 = DIRECTION ( 'NONE',  ( 0.000000000000000000, -0.000000000000000000, 1.000000000000000000 ) ) ;
#4811 = ADVANCED_FACE ( 'NONE', ( #4471 ), #5226, .T. ) ;
#4812 = CARTESIAN_POINT ( 'NONE',  ( -0.5141614760841463072, 0.9609181420092333115, -1.361499588670821659 ) ) ;
#4813 = DIRECTION ( 'NONE',  ( 0.000000000000000000, 0.000000000000000000, 1.000000000000000000 ) ) ;
#4814 = DIRECTION ( 'NONE',  ( -1.047444401652940007E-14, 1.000000000000000000, -4.625929269271482167E-15 ) ) ;
#4815 = DIRECTION ( 'NONE',  ( 0.000000000000000000, 0.5000000000000008882, -0.8660254037844380415 ) ) ;
#4816 = CARTESIAN_POINT ( 'NONE',  ( 0.4333661275892078946, -1.041228047528454548, -1.574803149606299302 ) ) ;
#4817 = DIRECTION ( 'NONE',  ( -1.000000000000000000, 0.000000000000000000, 0.000000000000000000 ) ) ;
#4818 = VERTEX_POINT ( 'NONE', #1509 ) ;
#4819 = CARTESIAN_POINT ( 'NONE',  ( 0.000000000000000000, 0.000000000000000000, -1.484898342931014303 ) ) ;
#4820 = CARTESIAN_POINT ( 'NONE',  ( 0.3425764178929368020, -0.2322094954269898481, 0.2008802154383053373 ) ) ;
#4821 = VERTEX_POINT ( 'NONE', #3857 ) ;
#4822 = EDGE_CURVE ( 'NONE', #6856, #489, #4965, .T. ) ;
#4823 = ADVANCED_FACE ( 'NONE', ( #7439 ), #379, .F. ) ;
#4824 = EDGE_CURVE ( 'NONE', #1258, #1074, #462, .T. ) ;
#4825 = CARTESIAN_POINT ( 'NONE',  ( 0.4348450248026701215, 1.063161309294319512, -1.569784497862150241 ) ) ;
#4826 = ORIENTED_EDGE ( 'NONE', *, *, #6184, .T. ) ;
#4827 = DIRECTION ( 'NONE',  ( -0.000000000000000000, -1.000000000000000000, -0.000000000000000000 ) ) ;
#4828 = ORIENTED_EDGE ( 'NONE', *, *, #4664, .F. ) ;
#4829 = ORIENTED_EDGE ( 'NONE', *, *, #6781, .T. ) ;
#4830 = CARTESIAN_POINT ( 'NONE',  ( 0.3510872220067592364, -0.3295092824291515621, -0.01982436236955561690 ) ) ;
#4831 = SHAPE_DEFINITION_REPRESENTATION ( #2581, #5531 ) ;
#4832 = CARTESIAN_POINT ( 'NONE',  ( 0.3322368487464851805, -0.06186759433717738121, 0.2952755905511811330 ) ) ;
#4833 = VERTEX_POINT ( 'NONE', #3392 ) ;
#4834 = FACE_OUTER_BOUND ( 'NONE', #3733, .T. ) ;
#4835 = ORIENTED_EDGE ( 'NONE', *, *, #979, .T. ) ;
#4836 =( NAMED_UNIT ( * ) PLANE_ANGLE_UNIT ( ) SI_UNIT ( $, .RADIAN. ) );
#4837 = PRODUCT ( 'MAT-019 Puller', 'MAT-019 Puller', '', ( #4222 ) ) ;
#4838 = CARTESIAN_POINT ( 'NONE',  ( -0.4526810454163320840, 0.9044351468059372845, -1.447629383090424549 ) ) ;
#4839 = CARTESIAN_POINT ( 'NONE',  ( -1.080458485393813062, 0.4837908950006628572, -1.514208454829284234 ) ) ;
#4840 =( GEOMETRIC_REPRESENTATION_CONTEXT ( 3 ) GLOBAL_UNCERTAINTY_ASSIGNED_CONTEXT ( ( #2433 ) ) GLOBAL_UNIT_ASSIGNED_CONTEXT ( ( #7500, #4098, #1695 ) ) REPRESENTATION_CONTEXT ( 'NONE', 'WORKASPACE' ) );
#4841 = CARTESIAN_POINT ( 'NONE',  ( 0.4332776154273901836, -1.054581703806071413, -1.572814851683855819 ) ) ;
#4842 = DIRECTION ( 'NONE',  ( -1.000000000000000000, -0.000000000000000000, -0.000000000000000000 ) ) ;
#4843 = FACE_OUTER_BOUND ( 'NONE', #5111, .T. ) ;
#4844 = CARTESIAN_POINT ( 'NONE',  ( 1.070856907295301363, 0.4375700573520810432, -1.565644078513316551 ) ) ;
#4845 = CARTESIAN_POINT ( 'NONE',  ( 0.000000000000000000, 0.2557161625347750267, 0.1476377952755908163 ) ) ;
#4846 = CARTESIAN_POINT ( 'NONE',  ( 0.2066929133858267931, 0.000000000000000000, 0.1188976377952756375 ) ) ;
#4847 = DIRECTION ( 'NONE',  ( 0.000000000000000000, 0.000000000000000000, 1.000000000000000000 ) ) ;
#4848 = FACE_OUTER_BOUND ( 'NONE', #6998, .T. ) ;
#4849 = ORIENTED_EDGE ( 'NONE', *, *, #2020, .F. ) ;
#4850 = CARTESIAN_POINT ( 'NONE',  ( 0.3336175750056032951, -0.2273032555864670234, 0.1968503937007874682 ) ) ;
#4851 = ADVANCED_FACE ( 'NONE', ( #2665 ), #7362, .T. ) ;
#4852 = CARTESIAN_POINT ( 'NONE',  ( -0.4589126309195370457, 1.085572762089311416, -1.540322683979783003 ) ) ;
#4853 = ORIENTED_EDGE ( 'NONE', *, *, #1975, .F. ) ;
#4854 = CARTESIAN_POINT ( 'NONE',  ( 0.3442725010713152956, -0.1485386763991280168, -0.2952755905511810774 ) ) ;
#4855 = CARTESIAN_POINT ( 'NONE',  ( 0.1771653543307088463, -0.3068593950417300431, 7.886165872636028972E-17 ) ) ;
#4856 = VECTOR ( 'NONE', #3517, 39.37007874015748143 ) ;
#4857 = CARTESIAN_POINT ( 'NONE',  ( 0.02637295201093723881, -0.1704774416898505729, -0.2952755905511810774 ) ) ;
#4858 = ORIENTED_EDGE ( 'NONE', *, *, #3503, .T. ) ;
#4859 = CARTESIAN_POINT ( 'NONE',  ( 0.4445636273010810657, -1.003669596044584278, -1.568530023225017223 ) ) ;
#4860 = EDGE_CURVE ( 'NONE', #4225, #2266, #3149, .T. ) ;
#4861 = EDGE_CURVE ( 'NONE', #1258, #2932, #3898, .T. ) ;
#4862 = B_SPLINE_CURVE_WITH_KNOTS ( 'NONE', 3,
 ( #4702, #2333, #8, #6359, #584, #5826, #7036, #7000, #2940, #4603 ),
 .UNSPECIFIED., .F., .F.,
 ( 4, 2, 2, 2, 4 ),
 ( 0.000000000000000000, 0.0005494620090385951951, 0.001098924018077190390, 0.001648386027115785694, 0.002197848036154380780 ),
 .UNSPECIFIED. ) ;
#4863 = AXIS2_PLACEMENT_3D ( 'NONE', #1056, #6879, #5629 ) ;
#4864 = DIRECTION ( 'NONE',  ( -0.000000000000000000, -0.000000000000000000, 1.000000000000000000 ) ) ;
#4865 = ORIENTED_EDGE ( 'NONE', *, *, #2066, .T. ) ;
#4866 = ORIENTED_EDGE ( 'NONE', *, *, #6914, .F. ) ;
#4867 = EDGE_CURVE ( 'NONE', #6033, #3513, #5114, .T. ) ;
#4868 = CARTESIAN_POINT ( 'NONE',  ( 0.000000000000000000, 0.000000000000000000, 0.000000000000000000 ) ) ;
#4869 = SHAPE_DEFINITION_REPRESENTATION ( #270, #785 ) ;
#4870 = CONICAL_SURFACE ( 'NONE', #3896, 0.2952755905511810774, 1.047197551196600518 ) ;
#4871 = DIRECTION ( 'NONE',  ( -0.000000000000000000, 0.000000000000000000, -1.000000000000000000 ) ) ;
#4872 = CARTESIAN_POINT ( 'NONE',  ( 0.3403864257300880936, 0.2851194846584802489, 0.09670974744601845696 ) ) ;
#4873 = ORIENTED_EDGE ( 'NONE', *, *, #7183, .F. ) ;
#4874 = CARTESIAN_POINT ( 'NONE',  ( 1.081428707249772803, -0.4470331066954845167, -1.553789012478535403 ) ) ;
#4875 = ADVANCED_FACE ( 'NONE', ( #5084 ), #4429, .T. ) ;
#4876 = FACE_OUTER_BOUND ( 'NONE', #1039, .T. ) ;
#4877 = AXIS2_PLACEMENT_3D ( 'NONE', #5256, #3897, #6800 ) ;
#4878 = VERTEX_POINT ( 'NONE', #3318 ) ;
#4879 = CARTESIAN_POINT ( 'NONE',  ( 0.000000000000000000, 0.000000000000000000, 0.000000000000000000 ) ) ;
#4880 = SURFACE_STYLE_USAGE ( .BOTH. , #4958 ) ;
#4881 = CARTESIAN_POINT ( 'NONE',  ( 0.02637295201093707228, -0.1704774416898499345, 0.2952755905511811330 ) ) ;
#4882 = DIRECTION ( 'NONE',  ( -0.000000000000000000, -1.000000000000000000, -0.000000000000000000 ) ) ;
#4883 = CIRCLE ( 'NONE', #3294, 0.2362204724409448231 ) ;
#4884 = FACE_OUTER_BOUND ( 'NONE', #3674, .T. ) ;
#4885 = CARTESIAN_POINT ( 'NONE',  ( 0.3391892065151629332, -0.1136516277932332758, 0.2952755905511811885 ) ) ;
#4886 = CARTESIAN_POINT ( 'NONE',  ( 7.874015748031496287, 0.000000000000000000, 0.000000000000000000 ) ) ;
#4887 = CARTESIAN_POINT ( 'NONE',  ( 0.000000000000000000, 0.000000000000000000, -0.4082677165354330340 ) ) ;
#4888 = CARTESIAN_POINT ( 'NONE',  ( 0.4330708661417321248, -1.044891351410288216, -1.574550377471545692 ) ) ;
#4889 = CARTESIAN_POINT ( 'NONE',  ( 0.7480314960629922405, 1.220472440944881942, 2.952755905511811108 ) ) ;
#4890 = DIRECTION ( 'NONE',  ( 0.3420201433256623291, 0.000000000000000000, -0.9396926207859106484 ) ) ;
#4891 = VERTEX_POINT ( 'NONE', #5667 ) ;
#4892 = CARTESIAN_POINT ( 'NONE',  ( 0.3306743754077736130, -0.2557161625347754708, 0.1476377952755905387 ) ) ;
#4893 = CARTESIAN_POINT ( 'NONE',  ( 0.3505602286436571569, 0.3409548833797004797, 4.673058124370679309E-18 ) ) ;
#4894 = CARTESIAN_POINT ( 'NONE',  ( 0.002513486811083437498, 0.2845799557467908469, -0.09764423893321776127 ) ) ;
#4895 = CARTESIAN_POINT ( 'NONE',  ( -1.279527559055118280, 1.968503937007874072, 2.480314960629921295 ) ) ;
#4896 = AXIS2_PLACEMENT_3D ( 'NONE', #3128, #197, #2031 ) ;
#4897 = CARTESIAN_POINT ( 'NONE',  ( 0.7480314960629922405, 0.7480314960629921295, 0.4921259842519685179 ) ) ;
#4898 = VERTEX_POINT ( 'NONE', #3821 ) ;
#4899 = CARTESIAN_POINT ( 'NONE',  ( 0.3426144402833972147, 0.2318662757222082205, -0.2014770286013785050 ) ) ;
#4900 = AXIS2_PLACEMENT_3D ( 'NONE', #6804, #5744, #6272 ) ;
#4901 = ORIENTED_EDGE ( 'NONE', *, *, #3935, .T. ) ;
#4902 = ORIENTED_EDGE ( 'NONE', *, *, #3321, .T. ) ;
#4903 = DIRECTION ( 'NONE',  ( 0.000000000000000000, 0.000000000000000000, 1.000000000000000000 ) ) ;
#4904 = EDGE_CURVE ( 'NONE', #7446, #6349, #5764, .T. ) ;
#4905 = AXIS2_PLACEMENT_3D ( 'NONE', #2209, #5768, #7435 ) ;
#4906 = CARTESIAN_POINT ( 'NONE',  ( 0.7480314960629923515, 2.892866454678784449E-17, -1.377952755905512028 ) ) ;
#4907 = EDGE_LOOP ( 'NONE', ( #1072, #774, #4376, #6460, #3484, #4858, #7009, #6202, #3125, #6567, #3986 ) ) ;
#4908 = CARTESIAN_POINT ( 'NONE',  ( 0.9895437626942018561, -0.4843361811957641594, -1.389133361342958173 ) ) ;
#4909 = ORIENTED_EDGE ( 'NONE', *, *, #1438, .T. ) ;
#4910 = AXIS2_PLACEMENT_3D ( 'NONE', #6363, #4705, #1175 ) ;
#4911 = CARTESIAN_POINT ( 'NONE',  ( -0.3543307086614173596, -0.1713008003332314177, -0.3862250106401512451 ) ) ;
#4912 = EDGE_LOOP ( 'NONE', ( #4745, #7042, #3924, #1613 ) ) ;
#4913 = CARTESIAN_POINT ( 'NONE',  ( 0.000000000000000000, 0.2559055118110236116, 0.000000000000000000 ) ) ;
#4914 = CARTESIAN_POINT ( 'NONE',  ( -0.3543307086614173040, 0.2045729300278205931, -0.3766201741223081378 ) ) ;
#4915 = AXIS2_PLACEMENT_3D ( 'NONE', #1122, #6336, #3129 ) ;
#4916 = ORIENTED_EDGE ( 'NONE', *, *, #5476, .F. ) ;
#4917 = ADVANCED_FACE ( 'NONE', ( #3936 ), #6267, .F. ) ;
#4918 = EDGE_CURVE ( 'NONE', #161, #6172, #637, .T. ) ;
#4919 =( CONVERSION_BASED_UNIT ( 'INCH', #3074 ) LENGTH_UNIT ( ) NAMED_UNIT ( #3354 ) );
#4920 = CARTESIAN_POINT ( 'NONE',  ( 0.01834252172841625839, 0.1843865549457985864, -0.2711842997036481573 ) ) ;
#4921 = CARTESIAN_POINT ( 'NONE',  ( 1.140074190135267118, -0.1777047106289595946, -0.9680897379949867654 ) ) ;
#4922 = VECTOR ( 'NONE', #2816, 39.37007874015748143 ) ;
#4923 = CARTESIAN_POINT ( 'NONE',  ( 0.3581828924050323715, 0.1743168766271107895, -0.3019256869348722061 ) ) ;
#4924 = VECTOR ( 'NONE', #5998, 39.37007874015748143 ) ;
#4925 = CARTESIAN_POINT ( 'NONE',  ( 0.7480314960629922405, 1.220472440944881942, 0.4724409448818898127 ) ) ;
#4926 = CARTESIAN_POINT ( 'NONE',  ( 0.3997746709170348356, 0.000000000000000000, 0.000000000000000000 ) ) ;
#4927 = CARTESIAN_POINT ( 'NONE',  ( 0.02637295201093722841, 0.3409548833797004797, 3.882420715168025960E-18 ) ) ;
#4928 = B_SPLINE_CURVE_WITH_KNOTS ( 'NONE', 3,
 ( #2449, #6586, #81, #6999, #4174, #6515, #2407, #42, #6550, #4744, #1334, #7077, #1751, #3681, #1883, #1788, #4214, #5942 ),
 .UNSPECIFIED., .F., .F.,
 ( 4, 2, 2, 2, 2, 2, 2, 2, 4 ),
 ( -8.121667112567890505E-06, 0.0009422843086939710396, 0.001417487296597246807, 0.001892690284500522574, 0.002367893272403798557, 0.002843096260307074324, 0.003318299248210350525, 0.003555900742161984072, 0.003793502236113617618 ),
 .UNSPECIFIED. ) ;
#4929 = DIRECTION ( 'NONE',  ( 0.000000000000000000, 0.000000000000000000, 1.000000000000000000 ) ) ;
#4930 = DIRECTION ( 'NONE',  ( 3.491481338843133750E-15, -1.000000000000000000, -4.625929269271482167E-15 ) ) ;
#4931 = VERTEX_POINT ( 'NONE', #1810 ) ;
#4932 = CARTESIAN_POINT ( 'NONE',  ( -0.9883299873891312481, 0.4377664870282915177, -1.443420526770070600 ) ) ;
#4933 = CARTESIAN_POINT ( 'NONE',  ( -0.4837911690062416947, 1.080458355692614836, -1.514208178040841846 ) ) ;
#4934 = CIRCLE ( 'NONE', #6395, 0.1982677165354330695 ) ;
#4935 = EDGE_LOOP ( 'NONE', ( #4014, #1038, #4494, #2980 ) ) ;
#4936 = CARTESIAN_POINT ( 'NONE',  ( -1.678725927747302331E-16, 0.2411939993270974525, 0.1727909197870958202 ) ) ;
#4937 = DIRECTION ( 'NONE',  ( -1.000000000000000000, -1.224646799147353454E-16, 0.000000000000000000 ) ) ;
#4938 = B_SPLINE_CURVE_WITH_KNOTS ( 'NONE', 3,
 ( #6237, #6951, #468, #4010, #992, #5638 ),
 .UNSPECIFIED., .F., .F.,
 ( 4, 2, 4 ),
 ( 0.004466737480205772853, 0.006712681563759903200, 0.008958625647314033547 ),
 .UNSPECIFIED. ) ;
#4939 = CIRCLE ( 'NONE', #3719, 0.2362204724409455170 ) ;
#4940 = CYLINDRICAL_SURFACE ( 'NONE', #7294, 0.2362204724409449064 ) ;
#4941 = ORIENTED_EDGE ( 'NONE', *, *, #1639, .T. ) ;
#4942 = CARTESIAN_POINT ( 'NONE',  ( 0.000000000000000000, 0.000000000000000000, -1.515748031496062964 ) ) ;
#4943 = VERTEX_POINT ( 'NONE', #7507 ) ;
#4944 = TOROIDAL_SURFACE ( 'NONE', #2362, 0.2952755905511811885, 0.05905511811023622659 ) ;
#4945 = MECHANICAL_DESIGN_GEOMETRIC_PRESENTATION_REPRESENTATION (  '', ( #5694 ), #296 ) ;
#4946 = ORIENTED_EDGE ( 'NONE', *, *, #484, .T. ) ;
#4947 = PLANE ( 'NONE',  #3561 ) ;
#4948 = CARTESIAN_POINT ( 'NONE',  ( 0.003035684155427232581, -0.2268414356900468332, 0.1976502892253331478 ) ) ;
#4949 = VERTEX_POINT ( 'NONE', #6946 ) ;
#4950 = LINE ( 'NONE', #3147, #6700 ) ;
#4951 = ORIENTED_EDGE ( 'NONE', *, *, #7243, .T. ) ;
#4952 = DIRECTION ( 'NONE',  ( 1.000000000000000000, 3.472416505924284230E-15, -1.431704036288781660E-14 ) ) ;
#4953 = ORIENTED_EDGE ( 'NONE', *, *, #4112, .T. ) ;
#4954 = B_SPLINE_CURVE_WITH_KNOTS ( 'NONE', 3,
 ( #1158, #1904, #4234, #3474, #568, #2884, #5231, #2042, #2314 ),
 .UNSPECIFIED., .F., .F.,
 ( 4, 2, 1, 2, 4 ),
 ( 0.000000000000000000, 0.002165063509461098365, 0.004330127018922196730, 0.006495190528383293360, 0.008660254037844391725 ),
 .UNSPECIFIED. ) ;
#4955 = ADVANCED_FACE ( 'NONE', ( #6407 ), #5261, .F. ) ;
#4956 = ORIENTED_EDGE ( 'NONE', *, *, #1029, .T. ) ;
#4957 = DIRECTION ( 'NONE',  ( -0.000000000000000000, -0.000000000000000000, 1.000000000000000000 ) ) ;
#4958 = SURFACE_SIDE_STYLE ('',( #5659 ) ) ;
#4959 = CARTESIAN_POINT ( 'NONE',  ( 0.000000000000000000, 0.000000000000000000, -0.4072677165354330331 ) ) ;
#4960 = CARTESIAN_POINT ( 'NONE',  ( 0.7556634140584972403, 0.06154568813258620014, -0.9824437959648022467 ) ) ;
#4961 = EDGE_CURVE ( 'NONE', #2380, #5096, #6505, .T. ) ;
#4962 = ADVANCED_FACE ( 'NONE', ( #1666 ), #2832, .T. ) ;
#4963 = ADVANCED_FACE ( 'NONE', ( #6982 ), #538, .F. ) ;
#4964 = CARTESIAN_POINT ( 'NONE',  ( 0.4338950423154144254, 1.037563309807724821, -1.574803149606299302 ) ) ;
#4965 = CIRCLE ( 'NONE', #4863, 1.968503937007874072 ) ;
#4966 = CARTESIAN_POINT ( 'NONE',  ( 0.3336175750056031841, 0.2273032555864666071, -0.1968503937007874127 ) ) ;
#4967 = CARTESIAN_POINT ( 'NONE',  ( 1.037563309807720380, 0.4338950423154246394, -1.574803149606299302 ) ) ;
#4968 = ORIENTED_EDGE ( 'NONE', *, *, #4105, .F. ) ;
#4969 = PRODUCT_DEFINITION_SHAPE ( 'NONE', 'NONE',  #7540 ) ;
#4970 = CARTESIAN_POINT ( 'NONE',  ( -0.9895441027518994126, 0.4843356560173161518, -1.389133886014302321 ) ) ;
#4971 = CARTESIAN_POINT ( 'NONE',  ( 0.3574299024618897702, 0.3465649303883613364, 6.884133197150707104E-16 ) ) ;
#4972 = APPLICATION_CONTEXT ( 'automotive_design' ) ;
#4973 = ORIENTED_EDGE ( 'NONE', *, *, #5286, .T. ) ;
#4974 = DIRECTION ( 'NONE',  ( 0.000000000000000000, 1.000000000000000000, 0.000000000000000000 ) ) ;
#4975 = CARTESIAN_POINT ( 'NONE',  ( 0.3387180295041032907, -0.02886098700874997411, -0.2952755905511810219 ) ) ;
#4976 = CARTESIAN_POINT ( 'NONE',  ( 0.8785537298370084125, 0.4700904924197999990, -1.433776001880364470 ) ) ;
#4977 = EDGE_LOOP ( 'NONE', ( #4407, #3379, #5983, #4681, #7272 ) ) ;
#4978 = CARTESIAN_POINT ( 'NONE',  ( 0.4700904924197903956, 0.000000000000000000, -2.204724409448820754 ) ) ;
#4979 = ORIENTED_EDGE ( 'NONE', *, *, #2320, .F. ) ;
#4980 = CIRCLE ( 'NONE', #1305, 0.03543307086614165546 ) ;
#4981 = ORIENTED_EDGE ( 'NONE', *, *, #3280, .F. ) ;
#4982 = DIRECTION ( 'NONE',  ( 0.000000000000000000, 0.000000000000000000, 1.000000000000000000 ) ) ;
#4983 = CARTESIAN_POINT ( 'NONE',  ( 0.9895437626941933074, 0.4843361811957848651, -1.389133361342959949 ) ) ;
#4984 = CARTESIAN_POINT ( 'NONE',  ( -5.972582710757682675E-17, -0.2484822268960368286, 0.1601673393405688428 ) ) ;
#4985 = VERTEX_POINT ( 'NONE', #563 ) ;
#4986 = DIRECTION ( 'NONE',  ( -4.632546475182562680E-15, 0.000000000000000000, 1.000000000000000000 ) ) ;
#4987 = EDGE_LOOP ( 'NONE', ( #76, #7265, #3139, #5523 ) ) ;
#4988 = AXIS2_PLACEMENT_3D ( 'NONE', #7173, #308, #1943 ) ;
#4989 = CARTESIAN_POINT ( 'NONE',  ( 0.9530933633567026941, 0.2342849080887553226, 0.9559618965236083010 ) ) ;
#4990 = VERTEX_POINT ( 'NONE', #2881 ) ;
#4991 = CARTESIAN_POINT ( 'NONE',  ( 0.2362204724409449619, 2.892866454678788147E-17, -0.4072677165354330331 ) ) ;
#4992 = VERTEX_POINT ( 'NONE', #5301 ) ;
#4993 = ORIENTED_EDGE ( 'NONE', *, *, #4766, .F. ) ;
#4994 = AXIS2_PLACEMENT_3D ( 'NONE', #5910, #3528, #1178 ) ;
#4995 = CARTESIAN_POINT ( 'NONE',  ( 25.35842062421581389, 45.20863634146751764, 54.13003647711799715 ) ) ;
#4996 = DIRECTION ( 'NONE',  ( -0.000000000000000000, -0.000000000000000000, 1.000000000000000000 ) ) ;
#4997 = EDGE_CURVE ( 'NONE', #2089, #2327, #6260, .T. ) ;
#4998 = CARTESIAN_POINT ( 'NONE',  ( 1.377952755905512028, 0.7480314960629921295, -0.7480314960629921295 ) ) ;
#4999 = VECTOR ( 'NONE', #671, 39.37007874015748143 ) ;
#5000 = CARTESIAN_POINT ( 'NONE',  ( 1.968503937007874072, 0.000000000000000000, 0.000000000000000000 ) ) ;
#5001 = CARTESIAN_POINT ( 'NONE',  ( 0.3483227611829846637, -0.1704774416898499345, 0.2952755905511811330 ) ) ;
#5002 = ADVANCED_FACE ( 'NONE', ( #4612 ), #599, .T. ) ;
#5003 = EDGE_CURVE ( 'NONE', #6730, #2124, #3538, .T. ) ;
#5004 = CARTESIAN_POINT ( 'NONE',  ( 0.4388996395293570663, 0.9346850374427945196, -1.455943645409046638 ) ) ;
#5005 = CARTESIAN_POINT ( 'NONE',  ( 7.874015748031496287, 0.2559055118110236116, 0.4921259842519685179 ) ) ;
#5006 = DIRECTION ( 'NONE',  ( 0.000000000000000000, -0.000000000000000000, 1.000000000000000000 ) ) ;
#5007 = CARTESIAN_POINT ( 'NONE',  ( 0.000000000000000000, 0.000000000000000000, 0.1188976377952756375 ) ) ;
#5008 = ORIENTED_EDGE ( 'NONE', *, *, #3793, .F. ) ;
#5009 = CARTESIAN_POINT ( 'NONE',  ( 0.4685039370078740717, 0.1704774416898497680, -0.2952755905511810774 ) ) ;
#5010 = EDGE_CURVE ( 'NONE', #6130, #4891, #6376, .T. ) ;
#5011 = VECTOR ( 'NONE', #3234, 39.37007874015748143 ) ;
#5012 = ORIENTED_EDGE ( 'NONE', *, *, #2854, .F. ) ;
#5013 = CARTESIAN_POINT ( 'NONE',  ( 0.000000000000000000, 0.2559055118110236116, -0.2362204724409449341 ) ) ;
#5014 = B_SPLINE_CURVE_WITH_KNOTS ( 'NONE', 3,
 ( #1042, #5645, #1102, #3414, #445, #5754, #4563, #401, #4487 ),
 .UNSPECIFIED., .F., .F.,
 ( 4, 2, 1, 2, 4 ),
 ( 0.000000000000000000, 0.002165063509461097064, 0.004330127018922194128, 0.006495190528383291625, 0.008660254037844388256 ),
 .UNSPECIFIED. ) ;
#5015 = DIRECTION ( 'NONE',  ( 0.000000000000000000, -1.000000000000000000, 0.000000000000000000 ) ) ;
#5016 = ADVANCED_FACE ( 'NONE', ( #7018 ), #5773, .F. ) ;
#5017 = APPLICATION_PROTOCOL_DEFINITION ( 'draft international standard', 'automotive_design', 1998, #6055 ) ;
#5018 = EDGE_CURVE ( 'NONE', #811, #1871, #3565, .T. ) ;
#5019 = MECHANICAL_DESIGN_GEOMETRIC_PRESENTATION_REPRESENTATION (  '', ( #6717 ), #507 ) ;
#5020 = CARTESIAN_POINT ( 'NONE',  ( 0.7480314960629923515, 1.544184662414706467E-22, 0.9842519685039370358 ) ) ;
#5021 = ORIENTED_EDGE ( 'NONE', *, *, #7378, .T. ) ;
#5022 = CARTESIAN_POINT ( 'NONE',  ( 0.000000000000000000, 0.000000000000000000, 0.1783464566929134354 ) ) ;
#5023 = ORIENTED_EDGE ( 'NONE', *, *, #3118, .T. ) ;
#5024 = EDGE_LOOP ( 'NONE', ( #2233, #7066 ) ) ;
#5025 = DIRECTION ( 'NONE',  ( 0.000000000000000000, 0.000000000000000000, -1.000000000000000000 ) ) ;
#5026 = CARTESIAN_POINT ( 'NONE',  ( 0.3585569128062318645, 0.1733077889112127901, 0.3036897776982951380 ) ) ;
#5027 = VERTEX_POINT ( 'NONE', #61 ) ;
#5028 =( GEOMETRIC_REPRESENTATION_CONTEXT ( 3 ) GLOBAL_UNCERTAINTY_ASSIGNED_CONTEXT ( ( #4708 ) ) GLOBAL_UNIT_ASSIGNED_CONTEXT ( ( #3228, #7351, #2689 ) ) REPRESENTATION_CONTEXT ( 'NONE', 'WORKASPACE' ) );
#5029 = CARTESIAN_POINT ( 'NONE',  ( 0.3483227611829846082, 0.1704774416898497680, -0.2952755905511810774 ) ) ;
#5030 = B_SPLINE_CURVE_WITH_KNOTS ( 'NONE', 3,
 ( #3122, #4816, #4888, #1986 ),
 .UNSPECIFIED., .F., .F.,
 ( 4, 4 ),
 ( 6.938893903907228378E-18, 0.0002807012396509388046 ),
 .UNSPECIFIED. ) ;
#5031 = EDGE_LOOP ( 'NONE', ( #2925, #2609, #2730, #7458 ) ) ;
#5032 = CARTESIAN_POINT ( 'NONE',  ( -0.5118110236220474452, 1.220472440944881942, 2.480314960629921295 ) ) ;
#5033 = DIRECTION ( 'NONE',  ( 1.000000000000000000, 0.000000000000000000, 0.000000000000000000 ) ) ;
#5034 = ORIENTED_EDGE ( 'NONE', *, *, #3369, .T. ) ;
#5035 = AXIS2_PLACEMENT_3D ( 'NONE', #5131, #3945, #4552 ) ;
#5036 = CARTESIAN_POINT ( 'NONE',  ( 2.989606299212598017, 0.000000000000000000, 0.000000000000000000 ) ) ;
#5037 = DIRECTION ( 'NONE',  ( -0.4186275392765909653, 0.9081580167345473242, 0.000000000000000000 ) ) ;
#5038 = AXIS2_PLACEMENT_3D ( 'NONE', #6441, #2957, #2466 ) ;
#5039 = DIRECTION ( 'NONE',  ( -0.000000000000000000, -1.000000000000000000, -0.000000000000000000 ) ) ;
#5040 = FACE_OUTER_BOUND ( 'NONE', #4176, .T. ) ;
#5041 = DIRECTION ( 'NONE',  ( 1.000000000000000000, 1.047067131017167108E-14, 0.000000000000000000 ) ) ;
#5042 = AXIS2_PLACEMENT_3D ( 'NONE', #2911, #2844, #5915 ) ;
#5043 = DIRECTION ( 'NONE',  ( 0.000000000000000000, 1.000000000000000000, 0.000000000000000000 ) ) ;
#5044 = CARTESIAN_POINT ( 'NONE',  ( 0.7511002112796222319, 0.03873617871155973086, -0.9835188775901014813 ) ) ;
#5045 = CARTESIAN_POINT ( 'NONE',  ( 0.4544645342395077225, 0.9861598787149296053, -1.560495034967182448 ) ) ;
#5046 = CIRCLE ( 'NONE', #2337, 1.223643328182681511 ) ;
#5047 = CARTESIAN_POINT ( 'NONE',  ( -6.322734125961233610E-17, -0.2702383257424528229, 0.1224846707640861176 ) ) ;
#5048 = CARTESIAN_POINT ( 'NONE',  ( 0.3496875272944827695, -0.1667004943313752652, 0.3018174552735723437 ) ) ;
#5049 = DIRECTION ( 'NONE',  ( -1.000000000000000000, -0.000000000000000000, -0.000000000000000000 ) ) ;
#5050 = CYLINDRICAL_SURFACE ( 'NONE', #1851, 1.968503937007874072 ) ;
#5051 = AXIS2_PLACEMENT_3D ( 'NONE', #162, #5236, #1129 ) ;
#5052 = EDGE_CURVE ( 'NONE', #6807, #2932, #3077, .T. ) ;
#5053 = CARTESIAN_POINT ( 'NONE',  ( 0.4330708661417324024, 5.520553484345353405E-17, -0.4507874015748032370 ) ) ;
#5054 = CARTESIAN_POINT ( 'NONE',  ( -0.7480314960629922405, 1.220472440944881942, 0.000000000000000000 ) ) ;
#5055 = PRODUCT_CONTEXT ( 'NONE', #673, 'mechanical' ) ;
#5056 = CARTESIAN_POINT ( 'NONE',  ( 0.1771653543307088463, 0.3068593950417300431, 7.886165872636028972E-17 ) ) ;
#5057 = ORIENTED_EDGE ( 'NONE', *, *, #51, .F. ) ;
#5058 = CARTESIAN_POINT ( 'NONE',  ( 1.063161309294324175, -0.4348450248026589637, -1.569784497862150907 ) ) ;
#5059 = CARTESIAN_POINT ( 'NONE',  ( 0.000000000000000000, 0.000000000000000000, -0.9857285720115422922 ) ) ;
#5060 = ADVANCED_FACE ( 'NONE', ( #4149 ), #26, .T. ) ;
#5061 = EDGE_CURVE ( 'NONE', #2732, #3522, #5412, .T. ) ;
#5062 = ORIENTED_EDGE ( 'NONE', *, *, #6837, .F. ) ;
#5063 = ORIENTED_EDGE ( 'NONE', *, *, #2578, .T. ) ;
#5064 = VECTOR ( 'NONE', #4761, 39.37007874015748143 ) ;
#5065 = EDGE_CURVE ( 'NONE', #5707, #6705, #2115, .T. ) ;
#5066 = EDGE_LOOP ( 'NONE', ( #2490, #6178 ) ) ;
#5067 = DIRECTION ( 'NONE',  ( -0.000000000000000000, -1.000000000000000000, -0.000000000000000000 ) ) ;
#5068 = ORIENTED_EDGE ( 'NONE', *, *, #2199, .T. ) ;
#5069 = DIRECTION ( 'NONE',  ( 0.000000000000000000, 0.000000000000000000, -1.000000000000000000 ) ) ;
#5070 = EDGE_LOOP ( 'NONE', ( #1375, #1647 ) ) ;
#5071 = VECTOR ( 'NONE', #1370, 39.37007874015748143 ) ;
#5072 = CARTESIAN_POINT ( 'NONE',  ( -3.198568410424924124, 2.407012729153881203, 0.4724409448818898127 ) ) ;
#5073 = ORIENTED_EDGE ( 'NONE', *, *, #3070, .T. ) ;
#5074 = DIMENSIONAL_EXPONENTS ( 1.000000000000000000, 0.000000000000000000, 0.000000000000000000, 0.000000000000000000, 0.000000000000000000, 0.000000000000000000, 0.000000000000000000 ) ;
#5075 = CARTESIAN_POINT ( 'NONE',  ( -1.781909941321919274E-15, 0.000000000000000000, -1.397637795275591843 ) ) ;
#5076 = DIRECTION ( 'NONE',  ( -1.000000000000000000, -1.972152263052529514E-31, -4.151318482771456951E-16 ) ) ;
#5077 = DIRECTION ( 'NONE',  ( 0.000000000000000000, 0.000000000000000000, 1.000000000000000000 ) ) ;
#5078 = CYLINDRICAL_SURFACE ( 'NONE', #1204, 0.2362204724409448231 ) ;
#5079 = CARTESIAN_POINT ( 'NONE',  ( 0.7480314960629923515, 1.205359478595430764E-16, -0.9842519685039370358 ) ) ;
#5080 = CARTESIAN_POINT ( 'NONE',  ( 0.1171731013849879183, 0.3414959384292343136, -0.4052515342986937608 ) ) ;
#5081 = CARTESIAN_POINT ( 'NONE',  ( 1.045688647185073705, 0.2282227683634086846, -0.9574297281001666882 ) ) ;
#5082 = CARTESIAN_POINT ( 'NONE',  ( 0.1171731013849879460, 0.3414959384292343136, -0.003016182236739221607 ) ) ;
#5083 = CARTESIAN_POINT ( 'NONE',  ( -2.834645669291338432, 0.4724409448818890911, 2.480314960629921295 ) ) ;
#5084 = FACE_OUTER_BOUND ( 'NONE', #1211, .T. ) ;
#5085 = CARTESIAN_POINT ( 'NONE',  ( -0.4700904924197908397, -0.8785537298370134085, -1.433776001880364470 ) ) ;
#5086 = ORIENTED_EDGE ( 'NONE', *, *, #249, .F. ) ;
#5087 = CARTESIAN_POINT ( 'NONE',  ( 2.834645669291338876, 0.4724409448818890911, 2.952755905511811108 ) ) ;
#5088 = ORIENTED_EDGE ( 'NONE', *, *, #1825, .T. ) ;
#5089 = DIRECTION ( 'NONE',  ( 0.000000000000000000, 0.000000000000000000, 1.000000000000000000 ) ) ;
#5090 = DIRECTION ( 'NONE',  ( -1.000000000000000000, 0.000000000000000000, 0.000000000000000000 ) ) ;
#5091 = CARTESIAN_POINT ( 'NONE',  ( -0.9984401429152544027, -0.4637690556582386714, -1.410743228759552048 ) ) ;
#5092 = VERTEX_POINT ( 'NONE', #6211 ) ;
#5093 = CARTESIAN_POINT ( 'NONE',  ( 0.3403864257301138507, 0.2263128404110440195, -0.1985658431051529893 ) ) ;
#5094 = AXIS2_PLACEMENT_3D ( 'NONE', #6430, #4750, #2873 ) ;
#5095 = CARTESIAN_POINT ( 'NONE',  ( 0.3337354549120238878, -0.2261274626982048841, 0.1988869267224354920 ) ) ;
#5096 = VERTEX_POINT ( 'NONE', #5610 ) ;
#5097 = ORIENTED_EDGE ( 'NONE', *, *, #1811, .T. ) ;
#5098 = CARTESIAN_POINT ( 'NONE',  ( 0.0006233585804810778822, -0.2702164766613439628, -0.1225225144826657953 ) ) ;
#5099 = FACE_OUTER_BOUND ( 'NONE', #2836, .T. ) ;
#5100 = EDGE_CURVE ( 'NONE', #662, #7286, #292, .T. ) ;
#5101 = CARTESIAN_POINT ( 'NONE',  ( 0.000000000000000000, 0.000000000000000000, -2.204724409448820754 ) ) ;
#5102 = ORIENTED_EDGE ( 'NONE', *, *, #4256, .F. ) ;
#5103 = EDGE_CURVE ( 'NONE', #5576, #345, #3449, .T. ) ;
#5104 = DIRECTION ( 'NONE',  ( 0.000000000000000000, 0.000000000000000000, -1.000000000000000000 ) ) ;
#5105 = EDGE_LOOP ( 'NONE', ( #1746, #4095, #1479 ) ) ;
#5106 = DIRECTION ( 'NONE',  ( -1.000000000000000000, 0.000000000000000000, 0.000000000000000000 ) ) ;
#5107 = AXIS2_PLACEMENT_3D ( 'NONE', #214, #5533, #3185 ) ;
#5108 = LINE ( 'NONE', #5032, #1711 ) ;
#5109 = EDGE_CURVE ( 'NONE', #4172, #5128, #7386, .T. ) ;
#5110 = VERTEX_POINT ( 'NONE', #7349 ) ;
#5111 = EDGE_LOOP ( 'NONE', ( #2942, #3569 ) ) ;
#5112 = CARTESIAN_POINT ( 'NONE',  ( 0.9659644734970493918, 0.4700904924198003876, -1.546597720061112069 ) ) ;
#5113 = DIRECTION ( 'NONE',  ( -0.4978050506594153823, -0.8672889550420767035, 9.730114419420828034E-16 ) ) ;
#5114 = CIRCLE ( 'NONE', #1612, 0.2699662542182227343 ) ;
#5115 = CARTESIAN_POINT ( 'NONE',  ( 0.4330708661417324024, 0.000000000000000000, 0.000000000000000000 ) ) ;
#5116 = EDGE_CURVE ( 'NONE', #2119, #1248, #820, .T. ) ;
#5117 = CARTESIAN_POINT ( 'NONE',  ( 0.000000000000000000, 2.892866454678787531E-17, -0.2362204724409449064 ) ) ;
#5118 = DIRECTION ( 'NONE',  ( 1.000000000000000000, -1.224646799147353207E-16, 0.000000000000000000 ) ) ;
#5119 = CONICAL_SURFACE ( 'NONE', #7055, 0.3543307086614173596, 1.047197551196596521 ) ;
#5120 = CARTESIAN_POINT ( 'NONE',  ( 0.1469816153540864645, 0.3242859848650326282, 2.518422369159242870E-16 ) ) ;
#5121 =( REPRESENTATION_RELATIONSHIP ('NONE','NONE', #303, #5265 ) REPRESENTATION_RELATIONSHIP_WITH_TRANSFORMATION ( #7104 )SHAPE_REPRESENTATION_RELATIONSHIP( ) );
#5122 = DIRECTION ( 'NONE',  ( -0.000000000000000000, -0.000000000000000000, -1.000000000000000000 ) ) ;
#5123 = VECTOR ( 'NONE', #4078, 39.37007874015748143 ) ;
#5124 = CARTESIAN_POINT ( 'NONE',  ( 0.3565422270302656127, -0.1673297761639321035, 0.3007275071673038980 ) ) ;
#5125 = DIRECTION ( 'NONE',  ( -0.000000000000000000, -1.000000000000000000, -0.000000000000000000 ) ) ;
#5126 = CARTESIAN_POINT ( 'NONE',  ( -0.4559220466128923732, -0.8989365377700720972, -1.445239289764782775 ) ) ;
#5127 = CARTESIAN_POINT ( 'NONE',  ( -0.2699662542182227343, 3.306133091061471023E-17, 0.1188976377952756375 ) ) ;
#5128 = VERTEX_POINT ( 'NONE', #1968 ) ;
#5129 = AXIS2_PLACEMENT_3D ( 'NONE', #732, #3054, #5404 ) ;
#5130 = FACE_BOUND ( 'NONE', #3447, .T. ) ;
#5131 = CARTESIAN_POINT ( 'NONE',  ( 0.4685039370078740717, 0.000000000000000000, 0.000000000000000000 ) ) ;
#5132 = ITEM_DEFINED_TRANSFORMATION ( 'NONE', 'NONE', #1352,  #5166 ) ;
#5133 = CARTESIAN_POINT ( 'NONE',  ( -0.2831409772408586822, 0.000000000000000000, -0.8561751947315059397 ) ) ;
#5134 = ORIENTED_EDGE ( 'NONE', *, *, #701, .T. ) ;
#5135 = CARTESIAN_POINT ( 'NONE',  ( 0.3387177083556421331, 0.2412911239081777792, -0.1726226950780199998 ) ) ;
#5136 = VECTOR ( 'NONE', #1238, 39.37007874015748143 ) ;
#5137 = CARTESIAN_POINT ( 'NONE',  ( 0.3585665126877354281, 0.1732820025503171713, -0.3037348580927971553 ) ) ;
#5138 = ORIENTED_EDGE ( 'NONE', *, *, #1147, .T. ) ;
#5139 = EDGE_LOOP ( 'NONE', ( #1337, #2159, #7350, #128 ) ) ;
#5140 = CARTESIAN_POINT ( 'NONE',  ( 1.214400861842334090, -0.05376942629958520597, 0.9828113691670130603 ) ) ;
#5141 = AXIS2_PLACEMENT_3D ( 'NONE', #3422, #905, #6751 ) ;
#5142 = CARTESIAN_POINT ( 'NONE',  ( 0.9696319393316025215, 0.5073702590876725260, -1.367288630522124793 ) ) ;
#5143 = DIRECTION ( 'NONE',  ( -1.000000000000000000, -0.000000000000000000, -0.000000000000000000 ) ) ;
#5144 = ORIENTED_EDGE ( 'NONE', *, *, #3092, .F. ) ;
#5145 = CARTESIAN_POINT ( 'NONE',  ( 0.3574299024618896037, 0.1732824651941676231, 0.3001340337771135625 ) ) ;
#5146 = VERTEX_POINT ( 'NONE', #7270 ) ;
#5147 = B_SPLINE_CURVE_WITH_KNOTS ( 'NONE', 3,
 ( #4714, #632, #4480, #4609, #4037, #7047, #6370, #6480 ),
 .UNSPECIFIED., .F., .F.,
 ( 4, 2, 2, 4 ),
 ( -7.690028535486425530E-06, 0.001102852776893263782, 0.001658124179607642096, 0.002213395582322020411 ),
 .UNSPECIFIED. ) ;
#5148 = CYLINDRICAL_SURFACE ( 'NONE', #7225, 0.2362204724409449619 ) ;
#5149 = ORIENTED_EDGE ( 'NONE', *, *, #2388, .T. ) ;
#5150 = EDGE_CURVE ( 'NONE', #2222, #1896, #87, .T. ) ;
#5151 = ORIENTED_EDGE ( 'NONE', *, *, #6878, .F. ) ;
#5152 = DIRECTION ( 'NONE',  ( -1.000000000000000000, -0.000000000000000000, 0.000000000000000000 ) ) ;
#5153 = DIRECTION ( 'NONE',  ( -1.000000000000000000, -7.046558751726398440E-19, -3.899598398114372558E-16 ) ) ;
#5154 = CARTESIAN_POINT ( 'NONE',  ( 0.4685039370078740717, -0.1704774416898499345, 0.2952755905511811330 ) ) ;
#5155 = TOROIDAL_SURFACE ( 'NONE', #6121, 1.124634398195722973, 0.05905511811023622659 ) ;
#5156 = CARTESIAN_POINT ( 'NONE',  ( 0.3483227611829846082, 0.1704774416898497680, -0.2952755905511810774 ) ) ;
#5157 = CARTESIAN_POINT ( 'NONE',  ( -0.3543307086614173040, -0.2045729300278205653, -0.4082677165354330340 ) ) ;
#5158 = DIRECTION ( 'NONE',  ( -0.000000000000000000, -0.000000000000000000, 1.000000000000000000 ) ) ;
#5159 = CARTESIAN_POINT ( 'NONE',  ( -0.4330708661417317362, 1.048552902599920733, -1.573978973432617279 ) ) ;
#5160 = VECTOR ( 'NONE', #5267, 39.37007874015748143 ) ;
#5161 = EDGE_CURVE ( 'NONE', #2401, #3022, #6933, .T. ) ;
#5162 = EDGE_CURVE ( 'NONE', #4456, #6588, #191, .T. ) ;
#5163 = ADVANCED_FACE ( 'NONE', ( #2299 ), #5148, .F. ) ;
#5164 = TOROIDAL_SURFACE ( 'NONE', #6883, 1.043121362164705745, 0.05905511811023622659 ) ;
#5165 = CARTESIAN_POINT ( 'NONE',  ( 0.3410249605999410294, 1.062103031354818709E-12, 0.3014927230551906479 ) ) ;
#5166 = AXIS2_PLACEMENT_3D ( 'NONE', #418, #2134, #2741 ) ;
#5167 = DIRECTION ( 'NONE',  ( 1.000000000000000000, 0.000000000000000000, 0.000000000000000000 ) ) ;
#5168 = AXIS2_PLACEMENT_3D ( 'NONE', #2189, #1488, #5566 ) ;
#5169 = CARTESIAN_POINT ( 'NONE',  ( 0.000000000000000000, 0.000000000000000000, 0.000000000000000000 ) ) ;
#5170 = AXIS2_PLACEMENT_3D ( 'NONE', #2428, #6909, #2611 ) ;
#5171 = CARTESIAN_POINT ( 'NONE',  ( 0.02637295201093697167, 0.1704774416898497680, -0.2952755905511810774 ) ) ;
#5172 = CARTESIAN_POINT ( 'NONE',  ( 1.968503937007874072, 0.000000000000000000, -0.4921259842519685179 ) ) ;
#5173 = CARTESIAN_POINT ( 'NONE',  ( -0.9883299873891298049, -0.4377664870282987342, -1.443420526770072820 ) ) ;
#5174 = ORIENTED_EDGE ( 'NONE', *, *, #1199, .F. ) ;
#5175 = AXIS2_PLACEMENT_3D ( 'NONE', #5177, #7487, #3868 ) ;
#5176 = CARTESIAN_POINT ( 'NONE',  ( 0.3322361761492156895, 0.2866471735582875047, -0.09406371265339424914 ) ) ;
#5177 = CARTESIAN_POINT ( 'NONE',  ( -2.834645669291338432, 0.4724409448818890911, 8.169257281319195485 ) ) ;
#5178 = VERTEX_POINT ( 'NONE', #1106 ) ;
#5179 = AXIS2_PLACEMENT_3D ( 'NONE', #6681, #261, #2622 ) ;
#5180 = CARTESIAN_POINT ( 'NONE',  ( 0.7965081100895167188, -0.1441822837186601813, 0.9737193899100770045 ) ) ;
#5181 = CIRCLE ( 'NONE', #1879, 0.9964144355006142595 ) ;
#5182 = FILL_AREA_STYLE ('',( #1686 ) ) ;
#5183 = VERTEX_POINT ( 'NONE', #3997 ) ;
#5184 = CARTESIAN_POINT ( 'NONE',  ( 0.3483227611829846637, -0.1704774416898499345, 0.2952755905511811330 ) ) ;
#5185 = ORIENTED_EDGE ( 'NONE', *, *, #1153, .F. ) ;
#5186 = CARTESIAN_POINT ( 'NONE',  ( -0.3543307086614173040, -0.2045729300278205931, -0.3766201741223081378 ) ) ;
#5187 = FACE_BOUND ( 'NONE', #7399, .T. ) ;
#5188 = LINE ( 'NONE', #933, #3533 ) ;
#5189 = EDGE_LOOP ( 'NONE', ( #6056, #1064, #2318, #4125 ) ) ;
#5190 = DIRECTION ( 'NONE',  ( 1.000000000000000000, 0.000000000000000000, 0.000000000000000000 ) ) ;
#5191 = DIRECTION ( 'NONE',  ( 1.000000000000000000, 0.000000000000000000, 0.000000000000000000 ) ) ;
#5192 = DIRECTION ( 'NONE',  ( 1.000000000000000000, 0.000000000000000000, -0.000000000000000000 ) ) ;
#5193 = DIRECTION ( 'NONE',  ( -1.000000000000000000, -0.000000000000000000, -0.000000000000000000 ) ) ;
#5194 = CARTESIAN_POINT ( 'NONE',  ( -0.3543307086614173040, 0.1379824317933219802, -0.01414634932344258599 ) ) ;
#5195 = ADVANCED_FACE ( 'NONE', ( #3451 ), #4793, .T. ) ;
#5196 = CARTESIAN_POINT ( 'NONE',  ( 7.874015748031496287, 0.2559055118110236116, 0.000000000000000000 ) ) ;
#5197 = EDGE_CURVE ( 'NONE', #5932, #1529, #4549, .T. ) ;
#5198 = CARTESIAN_POINT ( 'NONE',  ( -2.834645669291338432, 0.4724409448818898127, 2.480314960629921295 ) ) ;
#5199 = ADVANCED_FACE ( 'NONE', ( #6250 ), #5543, .T. ) ;
#5200 = CARTESIAN_POINT ( 'NONE',  ( -0.8833361873720544377, 0.4663632139996183867, -1.436953241411863313 ) ) ;
#5201 = FACE_BOUND ( 'NONE', #3263, .T. ) ;
#5202 = ITEM_DEFINED_TRANSFORMATION ( 'NONE', 'NONE', #4651,  #5166 ) ;
#5203 = DIRECTION ( 'NONE',  ( 1.000000000000000000, 0.000000000000000000, 0.000000000000000000 ) ) ;
#5204 = ORIENTED_EDGE ( 'NONE', *, *, #2989, .F. ) ;
#5205 = CARTESIAN_POINT ( 'NONE',  ( 0.3398312250857989381, -0.1962691648279019652, 0.2506030156613254789 ) ) ;
#5206 = ORIENTED_EDGE ( 'NONE', *, *, #706, .F. ) ;
#5207 = EDGE_LOOP ( 'NONE', ( #1100, #6243, #2293, #6815, #2936, #1308 ) ) ;
#5208 = CARTESIAN_POINT ( 'NONE',  ( 1.089060247968624440, -0.2122540722833457794, 0.9611122372014845316 ) ) ;
#5209 = PRODUCT_DEFINITION_FORMATION_WITH_SPECIFIED_SOURCE ( 'ANY', '', #4837, .NOT_KNOWN. ) ;
#5210 = SURFACE_STYLE_FILL_AREA ( #5182 ) ;
#5211 = VERTEX_POINT ( 'NONE', #4025 ) ;
#5212 = CARTESIAN_POINT ( 'NONE',  ( 1.212838072735738848, 0.06155971505712520137, 0.9824432156515408021 ) ) ;
#5213 = CARTESIAN_POINT ( 'NONE',  ( 0.000000000000000000, 0.000000000000000000, 0.000000000000000000 ) ) ;
#5214 = ORIENTED_EDGE ( 'NONE', *, *, #5280, .F. ) ;
#5215 = DIMENSIONAL_EXPONENTS ( 1.000000000000000000, 0.000000000000000000, 0.000000000000000000, 0.000000000000000000, 0.000000000000000000, 0.000000000000000000, 0.000000000000000000 ) ;
#5216 =( REPRESENTATION_RELATIONSHIP ('NONE','NONE', #303, #2104 ) REPRESENTATION_RELATIONSHIP_WITH_TRANSFORMATION ( #1927 )SHAPE_REPRESENTATION_RELATIONSHIP( ) );
#5217 = ORIENTED_EDGE ( 'NONE', *, *, #7389, .T. ) ;
#5218 = CARTESIAN_POINT ( 'NONE',  ( 0.4700904924197906176, 0.9659644734970541657, -1.546597720061111847 ) ) ;
#5219 = B_SPLINE_CURVE_WITH_KNOTS ( 'NONE', 3,
 ( #7291, #2069, #1474, #3827, #6161, #5777, #3436, #1092 ),
 .UNSPECIFIED., .F., .F.,
 ( 4, 2, 2, 4 ),
 ( 0.005257893453559884557, 0.006567392922673222569, 0.007876892391786559713, 0.01049589133001323574 ),
 .UNSPECIFIED. ) ;
#5220 = CARTESIAN_POINT ( 'NONE',  ( 18.41860179314716461, 41.48855051017370243, 54.34893959946985831 ) ) ;
#5221 = DIRECTION ( 'NONE',  ( 0.000000000000000000, 0.000000000000000000, -1.000000000000000000 ) ) ;
#5222 = FILL_AREA_STYLE ('',( #6259 ) ) ;
#5223 = COLOUR_RGB ( '',0.7921568627450980005, 0.8196078431372548767, 0.9333333333333333481 ) ;
#5224 = FACE_OUTER_BOUND ( 'NONE', #2035, .T. ) ;
#5225 = DIRECTION ( 'NONE',  ( 0.000000000000000000, 0.5000000000000008882, -0.8660254037844380415 ) ) ;
#5226 = CONICAL_SURFACE ( 'NONE', #6210, 0.2952755905511810774, 1.047197551196600518 ) ;
#5227 = LINE ( 'NONE', #4150, #526 ) ;
#5228 = FACE_OUTER_BOUND ( 'NONE', #3800, .T. ) ;
#5229 = ADVANCED_FACE ( 'NONE', ( #4633 ), #3202, .T. ) ;
#5230 = EDGE_CURVE ( 'NONE', #1792, #1409, #3700, .T. ) ;
#5231 = CARTESIAN_POINT ( 'NONE',  ( 0.3391892065151629332, 0.3125419764313920323, 0.04921259842519686012 ) ) ;
#5232 = VECTOR ( 'NONE', #5067, 39.37007874015748143 ) ;
#5233 = EDGE_CURVE ( 'NONE', #322, #5027, #1008, .T. ) ;
#5234 = CARTESIAN_POINT ( 'NONE',  ( 0.3505602286436571013, -0.1704774416898497957, 0.2952755905511814660 ) ) ;
#5235 = ORIENTED_EDGE ( 'NONE', *, *, #7375, .F. ) ;
#5236 = DIRECTION ( 'NONE',  ( -0.000000000000000000, -1.000000000000000000, -0.000000000000000000 ) ) ;
#5237 = CARTESIAN_POINT ( 'NONE',  ( 2.834645669291338432, 0.000000000000000000, 2.952755905511811108 ) ) ;
#5238 = AXIS2_PLACEMENT_3D ( 'NONE', #1096, #544, #3866 ) ;
#5239 = ORIENTED_EDGE ( 'NONE', *, *, #1626, .T. ) ;
#5240 = EDGE_CURVE ( 'NONE', #6850, #3252, #409, .T. ) ;
#5241 = ORIENTED_EDGE ( 'NONE', *, *, #7332, .F. ) ;
#5242 = EDGE_CURVE ( 'NONE', #4225, #4172, #6757, .T. ) ;
#5243 = CARTESIAN_POINT ( 'NONE',  ( 1.205350347085700102, -0.08351947907094880996, 0.9807282671443031674 ) ) ;
#5244 = B_SPLINE_CURVE_WITH_KNOTS ( 'NONE', 3,
 ( #4239, #3822, #1510, #4472, #6230, #309, #267, #2027, #4432, #6157 ),
 .UNSPECIFIED., .F., .F.,
 ( 4, 2, 2, 2, 4 ),
 ( 3.469446951953614189E-18, 0.0005494620090385985561, 0.001098924018077193643, 0.001648386027115788730, 0.002197848036154383816 ),
 .UNSPECIFIED. ) ;
#5245 = CIRCLE ( 'NONE', #2910, 0.2362204724409449341 ) ;
#5246 = CARTESIAN_POINT ( 'NONE',  ( 0.3425764178929367465, 0.2322094954269895706, -0.2008802154383052541 ) ) ;
#5247 = VERTEX_POINT ( 'NONE', #6289 ) ;
#5248 = CARTESIAN_POINT ( 'NONE',  ( -0.3543307086614173040, 0.000000000000000000, 7.886165872636028972E-17 ) ) ;
#5249 = CARTESIAN_POINT ( 'NONE',  ( 0.3528822938286764188, -0.1453909600788099998, 0.3018098512751525853 ) ) ;
#5250 = ORIENTED_EDGE ( 'NONE', *, *, #936, .F. ) ;
#5251 = AXIS2_PLACEMENT_3D ( 'NONE', #3849, #3735, #7277 ) ;
#5252 = CARTESIAN_POINT ( 'NONE',  ( 2.834645669291338876, 0.4724409448818890911, 0.4724409448818898127 ) ) ;
#5253 = CARTESIAN_POINT ( 'NONE',  ( -0.3543307086614173040, 0.2045729300278205931, -0.3766201741223081378 ) ) ;
#5254 =( CONVERSION_BASED_UNIT ( 'INCH', #1265 ) LENGTH_UNIT ( ) NAMED_UNIT ( #4621 ) );
#5255 = CARTESIAN_POINT ( 'NONE',  ( 0.3496875412996344190, 0.1780314126850971457, 0.2952755905511810774 ) ) ;
#5256 = CARTESIAN_POINT ( 'NONE',  ( -6.829619984160658046E-17, 0.4091458600556405201, -0.4082677165354330340 ) ) ;
#5257 = DIRECTION ( 'NONE',  ( -0.000000000000000000, -0.000000000000000000, 1.000000000000000000 ) ) ;
#5258 = ORIENTED_EDGE ( 'NONE', *, *, #4462, .T. ) ;
#5259 = AXIS2_PLACEMENT_3D ( 'NONE', #2973, #6991, #1745 ) ;
#5260 = CARTESIAN_POINT ( 'NONE',  ( 0.3505601438611540277, -0.1704774416898505729, -0.2952755905511810774 ) ) ;
#5261 = PLANE ( 'NONE',  #1359 ) ;
#5262 = TOROIDAL_SURFACE ( 'NONE', #4167, 1.124634398195722973, 0.05905511811023622659 ) ;
#5263 = DIRECTION ( 'NONE',  ( 1.000000000000000000, 0.000000000000000000, 0.000000000000000000 ) ) ;
#5264 = CARTESIAN_POINT ( 'NONE',  ( 0.3561392902752972267, 0.1723302545757742221, 0.2984847566065203517 ) ) ;
#5265 = SHAPE_REPRESENTATION ( 'torque nut 09_iso_ISO 10512-M12x1.5-N', ( #5166 ), #6134 ) ;
#5266 = CARTESIAN_POINT ( 'NONE',  ( 0.4368170415251730332, -0.9411659768779424562, -1.456692913385826849 ) ) ;
#5267 = DIRECTION ( 'NONE',  ( -0.000000000000000000, -0.000000000000000000, 1.000000000000000000 ) ) ;
#5268 = CIRCLE ( 'NONE', #1228, 0.2362204724409448231 ) ;
#5269 = CARTESIAN_POINT ( 'NONE',  ( 1.377952755905512028, 0.7480314960629921295, -0.7480314960629921295 ) ) ;
#5270 = EDGE_LOOP ( 'NONE', ( #330, #56, #289, #5008, #6123 ) ) ;
#5271 = FACE_OUTER_BOUND ( 'NONE', #4144, .T. ) ;
#5272 = EDGE_CURVE ( 'NONE', #4833, #6892, #5290, .T. ) ;
#5273 = DIRECTION ( 'NONE',  ( 0.000000000000000000, 1.000000000000000000, 0.000000000000000000 ) ) ;
#5274 = VERTEX_POINT ( 'NONE', #2158 ) ;
#5275 = CARTESIAN_POINT ( 'NONE',  ( 0.8865586066401955900, -0.2152123167378564572, 0.9604399500593175931 ) ) ;
#5276 = AXIS2_PLACEMENT_3D ( 'NONE', #4942, #6020, #6124 ) ;
#5277 = DIRECTION ( 'NONE',  ( -0.000000000000000000, -1.000000000000000000, -0.000000000000000000 ) ) ;
#5278 = VERTEX_POINT ( 'NONE', #487 ) ;
#5279 = CARTESIAN_POINT ( 'NONE',  ( 0.3410249605999410294, -1.062517223525361548E-12, -0.3014927230551905368 ) ) ;
#5280 = EDGE_CURVE ( 'NONE', #4821, #3761, #4661, .T. ) ;
#5281 = EDGE_CURVE ( 'NONE', #6856, #5971, #4788, .T. ) ;
#5282 = CARTESIAN_POINT ( 'NONE',  ( -0.7480314960629922405, 1.220472440944881942, 0.4724409448818898127 ) ) ;
#5283 = DIRECTION ( 'NONE',  ( -0.000000000000000000, -0.000000000000000000, 1.000000000000000000 ) ) ;
#5284 = ORIENTED_EDGE ( 'NONE', *, *, #711, .F. ) ;
#5285 = AXIS2_PLACEMENT_3D ( 'NONE', #7046, #3534, #6401 ) ;
#5286 = EDGE_CURVE ( 'NONE', #2074, #1762, #3655, .T. ) ;
#5287 = DIRECTION ( 'NONE',  ( 0.000000000000000000, 0.000000000000000000, 1.000000000000000000 ) ) ;
#5288 = DIRECTION ( 'NONE',  ( -0.000000000000000000, -1.000000000000000000, -0.000000000000000000 ) ) ;
#5289 = APPLICATION_PROTOCOL_DEFINITION ( 'draft international standard', 'automotive_design', 1998, #7449 ) ;
#5290 = B_SPLINE_CURVE_WITH_KNOTS ( 'NONE', 3,
 ( #2267, #5723, #5823, #7385 ),
 .UNSPECIFIED., .F., .F.,
 ( 4, 4 ),
 ( 0.000000000000000000, 0.0004815725036528569316 ),
 .UNSPECIFIED. ) ;
#5291 = CARTESIAN_POINT ( 'NONE',  ( 0.002479217192759452203, -0.05744896992506681732, 0.2952755905511810774 ) ) ;
#5292 = CARTESIAN_POINT ( 'NONE',  ( 0.3543307086614173040, 0.06965032677943194805, -0.4052140698951960385 ) ) ;
#5293 = PRESENTATION_LAYER_ASSIGNMENT (  '', '', ( #6036 ) ) ;
#5294 = CARTESIAN_POINT ( 'NONE',  ( 0.3391892065151627111, 0.1988903486381581598, -0.2460629921259842312 ) ) ;
#5295 = DIRECTION ( 'NONE',  ( 0.000000000000000000, 0.000000000000000000, -1.000000000000000000 ) ) ;
#5296 = ORIENTED_EDGE ( 'NONE', *, *, #2060, .F. ) ;
#5297 =( CONVERSION_BASED_UNIT ( 'INCH', #7015 ) LENGTH_UNIT ( ) NAMED_UNIT ( #5215 ) );
#5298 = CIRCLE ( 'NONE', #2738, 0.7480314960629921295 ) ;
#5299 = CARTESIAN_POINT ( 'NONE',  ( -0.4330708661417322913, -0.9666437042230143772, -1.454455828411337359 ) ) ;
#5300 = DIRECTION ( 'NONE',  ( -0.000000000000000000, -0.000000000000000000, 1.000000000000000000 ) ) ;
#5301 = CARTESIAN_POINT ( 'NONE',  ( -0.9842519685039370358, 1.220472440944881942, 2.952755905511811108 ) ) ;
#5302 = CARTESIAN_POINT ( 'NONE',  ( -3.198568410424924124, 2.407012729153881203, 0.4724409448818898127 ) ) ;
#5303 = AXIS2_PLACEMENT_3D ( 'NONE', #5036, #2201, #4531 ) ;
#5304 = CARTESIAN_POINT ( 'NONE',  ( 0.4720886891211135694, -0.9960023578760571761, -1.401719942879699143 ) ) ;
#5305 = CARTESIAN_POINT ( 'NONE',  ( -0.4637694296357178780, 0.9984400756355462647, -1.410742812766316190 ) ) ;
#5306 = CARTESIAN_POINT ( 'NONE',  ( -1.041228047528454104, -0.4333661275892064513, -1.574803149606299302 ) ) ;
#5307 = DIRECTION ( 'NONE',  ( -0.000000000000000000, -0.000000000000000000, 1.000000000000000000 ) ) ;
#5308 = DIRECTION ( 'NONE',  ( -1.000000000000000000, -0.000000000000000000, -0.000000000000000000 ) ) ;
#5309 = CARTESIAN_POINT ( 'NONE',  ( 0.3306743754077736130, -0.2557161625347754708, 0.1476377952755905387 ) ) ;
#5310 = EDGE_LOOP ( 'NONE', ( #4265, #543, #1712 ) ) ;
#5311 = DIRECTION ( 'NONE',  ( -0.000000000000000000, -1.000000000000000000, -0.000000000000000000 ) ) ;
#5312 = B_SPLINE_CURVE_WITH_KNOTS ( 'NONE', 3,
 ( #6116, #1433, #2630, #4323, #4242, #4932, #1947, #347, #3169, #2065, #875, #1470, #6579, #4970, #4394, #4278, #2518, #196 ),
 .UNSPECIFIED., .F., .F.,
 ( 4, 2, 2, 2, 2, 2, 2, 2, 4 ),
 ( 0.000000000000000000, 0.0002385177155853817146, 0.0004770354311707634292, 0.0009540708623415151491, 0.001431106293512267140, 0.001908141724683019022, 0.002385177155853770471, 0.002862212587024523004, 0.003816283449366010723 ),
 .UNSPECIFIED. ) ;
#5313 = CARTESIAN_POINT ( 'NONE',  ( 2.834645669291338876, 0.4724409448818890911, 0.000000000000000000 ) ) ;
#5314 = ORIENTED_EDGE ( 'NONE', *, *, #2929, .F. ) ;
#5315 = CARTESIAN_POINT ( 'NONE',  ( 0.7484094839556201251, -0.01546318525790828929, 0.9841610390795200169 ) ) ;
#5316 = LINE ( 'NONE', #3597, #4856 ) ;
#5317 = EDGE_LOOP ( 'NONE', ( #6701, #1533, #7235, #3302 ) ) ;
#5318 = CARTESIAN_POINT ( 'NONE',  ( 0.000000000000000000, 0.000000000000000000, -0.4082677165354330340 ) ) ;
#5319 = B_SPLINE_CURVE_WITH_KNOTS ( 'NONE', 3,
 ( #6537, #5469, #4318, #265, #7137, #1279, #5968, #228, #6574 ),
 .UNSPECIFIED., .F., .F.,
 ( 4, 2, 1, 2, 4 ),
 ( 0.000000000000000000, 0.002165063509461096630, 0.004330127018922193260, 0.006495190528383289023, 0.008660254037844388256 ),
 .UNSPECIFIED. ) ;
#5320 = ORIENTED_EDGE ( 'NONE', *, *, #7091, .T. ) ;
#5321 = PRODUCT ( 'torque nut 09_iso_ISO 10512-M12x1.5-N', 'torque nut 09_iso_ISO 10512-M12x1.5-N', '', ( #5908 ) ) ;
#5322 = CARTESIAN_POINT ( 'NONE',  ( 0.3459463601586513781, -0.1956820507697304701, -0.2516199270400212851 ) ) ;
#5323 = DIRECTION ( 'NONE',  ( 1.000000000000000000, 0.000000000000000000, 0.000000000000000000 ) ) ;
#5324 = DIRECTION ( 'NONE',  ( 0.000000000000000000, 0.000000000000000000, 1.000000000000000000 ) ) ;
#5325 = EDGE_CURVE ( 'NONE', #5590, #2217, #5902, .T. ) ;
#5326 = ADVANCED_FACE ( 'NONE', ( #1212 ), #5776, .T. ) ;
#5327 = SURFACE_STYLE_USAGE ( .BOTH. , #2988 ) ;
#5328 = FACE_OUTER_BOUND ( 'NONE', #1047, .T. ) ;
#5329 = ORIENTED_EDGE ( 'NONE', *, *, #6315, .T. ) ;
#5330 = ADVANCED_FACE ( 'NONE', ( #7034 ), #1480, .T. ) ;
#5331 = DIRECTION ( 'NONE',  ( -0.000000000000000000, -1.000000000000000000, -0.000000000000000000 ) ) ;
#5332 = CYLINDRICAL_SURFACE ( 'NONE', #2105, 0.3543307086614172485 ) ;
#5333 = ORIENTED_EDGE ( 'NONE', *, *, #3644, .T. ) ;
#5334 = EDGE_CURVE ( 'NONE', #5614, #1378, #164, .T. ) ;
#5335 = CARTESIAN_POINT ( 'NONE',  ( 0.01171324505787584534, -0.3130206113228972131, -0.04838357847483532731 ) ) ;
#5336 = CARTESIAN_POINT ( 'NONE',  ( -1.083410641227607218, 0.4508656291625769419, -1.549345754620972349 ) ) ;
#5337 = DIRECTION ( 'NONE',  ( 1.000000000000000000, 1.047444401652940007E-14, 0.000000000000000000 ) ) ;
#5338 = CARTESIAN_POINT ( 'NONE',  ( 0.3403868552871069930, -0.05881191477760600722, -0.2952755905511810774 ) ) ;
#5339 = AXIS2_PLACEMENT_3D ( 'NONE', #856, #4408, #6065 ) ;
#5340 = UNCERTAINTY_MEASURE_WITH_UNIT (LENGTH_MEASURE( 1.000000000000000082E-05 ), #4919, 'distance_accuracy_value', 'NONE');
#5341 = CARTESIAN_POINT ( 'NONE',  ( 0.9810556462971108393, 0.4349192958999855696, -1.448591228719269042 ) ) ;
#5342 = CARTESIAN_POINT ( 'NONE',  ( 0.2362204724409449619, 0.000000000000000000, -0.9857285720115422922 ) ) ;
#5343 = CARTESIAN_POINT ( 'NONE',  ( -2.834645669291338432, 0.4724409448818898127, 2.480314960629921295 ) ) ;
#5344 = AXIS2_PLACEMENT_3D ( 'NONE', #6190, #4431, #2098 ) ;
#5345 = DIRECTION ( 'NONE',  ( -1.000000000000000000, 1.776356839400250465E-15, 0.000000000000000000 ) ) ;
#5346 = CARTESIAN_POINT ( 'NONE',  ( -0.4882975260543733764, -0.9867938558989116649, -1.385219839936553177 ) ) ;
#5347 = CARTESIAN_POINT ( 'NONE',  ( 0.3483227611829848303, 0.3409548833797004797, 0.000000000000000000 ) ) ;
#5348 = CARTESIAN_POINT ( 'NONE',  ( 0.2831409772408586822, -8.928484287076473300E-17, -0.8561751947315059397 ) ) ;
#5349 = ORIENTED_EDGE ( 'NONE', *, *, #3893, .T. ) ;
#5350 = DIRECTION ( 'NONE',  ( -1.000000000000000000, 0.000000000000000000, 0.000000000000000000 ) ) ;
#5351 = DIRECTION ( 'NONE',  ( -1.000000000000000000, 0.000000000000000000, 0.000000000000000000 ) ) ;
#5352 = ORIENTED_EDGE ( 'NONE', *, *, #604, .F. ) ;
#5353 = AXIS2_PLACEMENT_3D ( 'NONE', #113, #4276, #268 ) ;
#5354 = EDGE_LOOP ( 'NONE', ( #2839, #5102, #1766, #1148, #2187, #3899, #6710, #3791 ) ) ;
#5355 = CARTESIAN_POINT ( 'NONE',  ( 0.1470270249832138776, -0.3242597676034325582, -0.0007480297793126593165 ) ) ;
#5356 =( REPRESENTATION_RELATIONSHIP ('NONE','NONE', #303, #1307 ) REPRESENTATION_RELATIONSHIP_WITH_TRANSFORMATION ( #3606 )SHAPE_REPRESENTATION_RELATIONSHIP( ) );
#5357 = DIRECTION ( 'NONE',  ( -1.000000000000000000, 0.000000000000000000, 0.000000000000000000 ) ) ;
#5358 = ORIENTED_EDGE ( 'NONE', *, *, #5161, .F. ) ;
#5359 = AXIS2_PLACEMENT_3D ( 'NONE', #4201, #1240, #686 ) ;
#5360 = DIRECTION ( 'NONE',  ( 0.000000000000000000, 1.000000000000000000, -1.001543065824774208E-16 ) ) ;
#5361 = ORIENTED_EDGE ( 'NONE', *, *, #5949, .F. ) ;
#5362 = ORIENTED_EDGE ( 'NONE', *, *, #3542, .F. ) ;
#5363 = DIRECTION ( 'NONE',  ( 0.000000000000000000, 0.000000000000000000, -1.000000000000000000 ) ) ;
#5364 = AXIS2_PLACEMENT_3D ( 'NONE', #126, #7078, #1790 ) ;
#5365 = DIRECTION ( 'NONE',  ( 1.047444401652940007E-14, -1.000000000000000000, 4.625929269271482167E-15 ) ) ;
#5366 = PRODUCT_CONTEXT ( 'NONE', #3867, 'mechanical' ) ;
#5367 =( NAMED_UNIT ( * ) SI_UNIT ( $, .STERADIAN. ) SOLID_ANGLE_UNIT ( ) );
#5368 = CARTESIAN_POINT ( 'NONE',  ( 0.4685039370078740717, 0.3409548833797004797, 0.000000000000000000 ) ) ;
#5369 = ORIENTED_EDGE ( 'NONE', *, *, #5891, .T. ) ;
#5370 = CARTESIAN_POINT ( 'NONE',  ( 1.064252964791707168, -0.5072158114884506297, -1.491281854710054811 ) ) ;
#5371 = ORIENTED_EDGE ( 'NONE', *, *, #842, .F. ) ;
#5372 = VECTOR ( 'NONE', #4069, 39.37007874015748143 ) ;
#5373 = DIRECTION ( 'NONE',  ( -0.000000000000000000, 0.000000000000000000, -1.000000000000000000 ) ) ;
#5374 = EDGE_CURVE ( 'NONE', #6357, #1882, #5046, .T. ) ;
#5375 = B_SPLINE_CURVE_WITH_KNOTS ( 'NONE', 3,
 ( #482, #2153, #6929, #1570, #2798, #2867 ),
 .UNSPECIFIED., .F., .F.,
 ( 4, 2, 4 ),
 ( 2.380732026380333730E-07, 0.002190927868076681349, 0.004381617662950723809 ),
 .UNSPECIFIED. ) ;
#5376 = ORIENTED_EDGE ( 'NONE', *, *, #5762, .T. ) ;
#5377 = AXIS2_PLACEMENT_3D ( 'NONE', #2947, #6431, #5866 ) ;
#5378 = CARTESIAN_POINT ( 'NONE',  ( 0.3465694189147311421, -0.3147628225698668736, -0.04536598007755129891 ) ) ;
#5379 = DIRECTION ( 'NONE',  ( 0.000000000000000000, 0.000000000000000000, 1.000000000000000000 ) ) ;
#5380 = CARTESIAN_POINT ( 'NONE',  ( -1.056523642887404968, 0.5141614760841421994, -1.484898342931014525 ) ) ;
#5381 = CARTESIAN_POINT ( 'NONE',  ( 0.3410249605999410294, -1.062517223525361548E-12, -0.3014927230551905368 ) ) ;
#5382 = EDGE_CURVE ( 'NONE', #5648, #1882, #4928, .T. ) ;
#5383 = EDGE_CURVE ( 'NONE', #5720, #4020, #3208, .T. ) ;
#5384 = DIRECTION ( 'NONE',  ( -0.7071067811865496822, 8.659560562354906974E-17, -0.7071067811865453523 ) ) ;
#5385 = CARTESIAN_POINT ( 'NONE',  ( -0.4476001829033103285, 0.9971724964169985661, -1.429776958199370451 ) ) ;
#5386 = CARTESIAN_POINT ( 'NONE',  ( -0.7480314960629922405, 1.220472440944881942, 2.952755905511811108 ) ) ;
#5387 = CONTEXT_DEPENDENT_SHAPE_REPRESENTATION ( #6923, #1348 ) ;
#5388 = CARTESIAN_POINT ( 'NONE',  ( 1.081428707249763699, 0.4470331066955068322, -1.553789012478534737 ) ) ;
#5389 =( GEOMETRIC_REPRESENTATION_CONTEXT ( 3 ) GLOBAL_UNCERTAINTY_ASSIGNED_CONTEXT ( ( #1849 ) ) GLOBAL_UNIT_ASSIGNED_CONTEXT ( ( #3109, #1418, #3651 ) ) REPRESENTATION_CONTEXT ( 'NONE', 'WORKASPACE' ) );
#5390 = DIRECTION ( 'NONE',  ( 0.000000000000000000, 0.000000000000000000, -1.000000000000000000 ) ) ;
#5391 = B_SPLINE_CURVE_WITH_KNOTS ( 'NONE', 3,
 ( #2627, #7284, #157, #5969 ),
 .UNSPECIFIED., .F., .F.,
 ( 4, 4 ),
 ( 0.000000000000000000, 0.0002807012396509390756 ),
 .UNSPECIFIED. ) ;
#5392 = FACE_OUTER_BOUND ( 'NONE', #5270, .T. ) ;
#5393 = CARTESIAN_POINT ( 'NONE',  ( 0.3543307086614173596, 0.000000000000000000, -0.4082677165354330340 ) ) ;
#5394 = DIRECTION ( 'NONE',  ( -0.000000000000000000, -1.000000000000000000, -0.000000000000000000 ) ) ;
#5395 = ORIENTED_EDGE ( 'NONE', *, *, #5230, .F. ) ;
#5396 = PRODUCT_DEFINITION_SHAPE ( 'NONE', 'NONE',  #7528 ) ;
#5397 = FACE_OUTER_BOUND ( 'NONE', #2860, .T. ) ;
#5398 = CARTESIAN_POINT ( 'NONE',  ( 0.3528850351813196395, -0.1886720902358828833, 0.2768301761068310274 ) ) ;
#5399 = ORIENTED_EDGE ( 'NONE', *, *, #5938, .T. ) ;
#5400 = CIRCLE ( 'NONE', #4900, 1.089828288828796676 ) ;
#5401 = VECTOR ( 'NONE', #6589, 39.37007874015748143 ) ;
#5402 = CARTESIAN_POINT ( 'NONE',  ( 0.02890955082422775116, -0.3924549231051219778, -0.02201102547170776663 ) ) ;
#5403 = CARTESIAN_POINT ( 'NONE',  ( 0.2362204724409449341, 0.000000000000000000, -3.582716535433073002 ) ) ;
#5404 = DIRECTION ( 'NONE',  ( 0.000000000000000000, 0.000000000000000000, 1.000000000000000000 ) ) ;
#5405 = AXIS2_PLACEMENT_3D ( 'NONE', #4143, #631, #4680 ) ;
#5406 = ORIENTED_EDGE ( 'NONE', *, *, #6965, .F. ) ;
#5407 = AXIS2_PLACEMENT_3D ( 'NONE', #7169, #2546, #6572 ) ;
#5408 = CARTESIAN_POINT ( 'NONE',  ( 0.4330708661417322913, 0.000000000000000000, -2.204724409448820754 ) ) ;
#5409 = CIRCLE ( 'NONE', #2828, 0.2362204724409449341 ) ;
#5410 = ORIENTED_EDGE ( 'NONE', *, *, #2072, .F. ) ;
#5411 = EDGE_LOOP ( 'NONE', ( #1165, #4367, #3111, #3300, #5755 ) ) ;
#5412 = CIRCLE ( 'NONE', #7353, 1.074277634097406953 ) ;
#5413 = CARTESIAN_POINT ( 'NONE',  ( -0.9659644734970558311, 0.4700904924197872314, -1.546597720061112069 ) ) ;
#5414 = FACE_OUTER_BOUND ( 'NONE', #1717, .T. ) ;
#5415 = PRODUCT_CONTEXT ( 'NONE', #4437, 'mechanical' ) ;
#5416 = FACE_OUTER_BOUND ( 'NONE', #1035, .T. ) ;
#5417 = ORIENTED_EDGE ( 'NONE', *, *, #1486, .T. ) ;
#5418 = CARTESIAN_POINT ( 'NONE',  ( 1.070877566692234328, -0.4996355910473124773, -1.498503231159224791 ) ) ;
#5419 = EDGE_LOOP ( 'NONE', ( #974, #3759, #2679, #902, #5785 ) ) ;
#5420 = AXIS2_PLACEMENT_3D ( 'NONE', #2029, #5439, #4356 ) ;
#5421 = SHAPE_REPRESENTATION_RELATIONSHIP ( 'NONE' , 'NONE' ,  #1552, #6318 ) ;
#5422 = CIRCLE ( 'NONE', #2225, 0.2362204724409449619 ) ;
#5423 = PRODUCT_RELATED_PRODUCT_CATEGORY ( 'part', '', ( #5321 ) ) ;
#5424 = CARTESIAN_POINT ( 'NONE',  ( 0.3565325103478086954, -0.1673557731150450700, -0.3006824791271353603 ) ) ;
#5425 = CARTESIAN_POINT ( 'NONE',  ( 0.7796304418040825857, -0.1182802082656420201, -0.9771433015668254951 ) ) ;
#5426 = CARTESIAN_POINT ( 'NONE',  ( -0.9842519685039370358, 1.220472440944881942, 0.4724409448818898127 ) ) ;
#5427 = CARTESIAN_POINT ( 'NONE',  ( 1.218928898036171882, 0.03106543388645563800, -0.9838782854499440456 ) ) ;
#5428 = AXIS2_PLACEMENT_3D ( 'NONE', #6227, #307, #4505 ) ;
#5429 = CARTESIAN_POINT ( 'NONE',  ( 0.000000000000000000, 0.000000000000000000, 0.000000000000000000 ) ) ;
#5430 = DIRECTION ( 'NONE',  ( -0.000000000000000000, -1.000000000000000000, -0.000000000000000000 ) ) ;
#5431 = EDGE_CURVE ( 'NONE', #698, #5178, #734, .T. ) ;
#5432 = EDGE_CURVE ( 'NONE', #5600, #6027, #3194, .T. ) ;
#5433 = CARTESIAN_POINT ( 'NONE',  ( 1.070877566692223892, 0.4996355910473349038, -1.498503231159224791 ) ) ;
#5434 = CARTESIAN_POINT ( 'NONE',  ( 0.9842519685039370358, 1.220472440944881942, 0.4724409448818898127 ) ) ;
#5435 = DIRECTION ( 'NONE',  ( 0.000000000000000000, 0.000000000000000000, 1.000000000000000000 ) ) ;
#5436 = DIRECTION ( 'NONE',  ( -0.000000000000000000, -1.000000000000000000, -0.000000000000000000 ) ) ;
#5437 = CARTESIAN_POINT ( 'NONE',  ( 0.002513486811083454845, 0.2268523693227592619, 0.1976313516179636909 ) ) ;
#5438 = ORIENTED_EDGE ( 'NONE', *, *, #1974, .F. ) ;
#5439 = DIRECTION ( 'NONE',  ( 1.047444401652940007E-14, -1.000000000000000000, 0.000000000000000000 ) ) ;
#5440 = ADVANCED_FACE ( 'NONE', ( #3020 ), #2368, .F. ) ;
#5441 = CARTESIAN_POINT ( 'NONE',  ( 6.901988839087968355E-18, 0.4091458600556405201, -0.4082677165354330340 ) ) ;
#5442 = ORIENTED_EDGE ( 'NONE', *, *, #3984, .F. ) ;
#5443 = CARTESIAN_POINT ( 'NONE',  ( 0.3426148638729746843, -0.05855635169929876427, -0.3015406112749626777 ) ) ;
#5444 = CYLINDRICAL_SURFACE ( 'NONE', #7338, 0.2362204724409449341 ) ;
#5445 = EDGE_CURVE ( 'NONE', #6856, #772, #125, .T. ) ;
#5446 = DIRECTION ( 'NONE',  ( 0.000000000000000000, 0.000000000000000000, 1.000000000000000000 ) ) ;
#5447 = ORIENTED_EDGE ( 'NONE', *, *, #4588, .F. ) ;
#5448 = CARTESIAN_POINT ( 'NONE',  ( 0.3479980290964227452, 0.3208941761715193852, -0.04760384692076755769 ) ) ;
#5449 = EDGE_LOOP ( 'NONE', ( #7363, #2970, #553, #7089, #3457, #2771 ) ) ;
#5450 = ORIENTED_EDGE ( 'NONE', *, *, #4387, .F. ) ;
#5451 = DIRECTION ( 'NONE',  ( -0.000000000000000000, -1.000000000000000000, -0.000000000000000000 ) ) ;
#5452 = APPLICATION_PROTOCOL_DEFINITION ( 'draft international standard', 'automotive_design', 1998, #286 ) ;
#5453 = CARTESIAN_POINT ( 'NONE',  ( 0.3581828924050327045, -0.3486337532542230222, -1.123169198254405176E-18 ) ) ;
#5454 = CARTESIAN_POINT ( 'NONE',  ( 0.3388536909603142577, 0.2250264928541962084, 0.2007938624298919450 ) ) ;
#5455 = ORIENTED_EDGE ( 'NONE', *, *, #4256, .T. ) ;
#5456 = CARTESIAN_POINT ( 'NONE',  ( 1.084813347358868363, -0.4713815370807298843, -1.526966122205014598 ) ) ;
#5457 = DIRECTION ( 'NONE',  ( 0.000000000000000000, 0.000000000000000000, 1.000000000000000000 ) ) ;
#5458 = EDGE_LOOP ( 'NONE', ( #4799, #2677 ) ) ;
#5459 = SHAPE_REPRESENTATION_RELATIONSHIP ( 'NONE' , 'NONE' ,  #7075, #314 ) ;
#5460 = PRODUCT_DEFINITION_SHAPE ( 'NONE', 'NONE',  #7523 ) ;
#5461 = CARTESIAN_POINT ( 'NONE',  ( 0.3496875272944831026, -0.3447318307381757041, 0.006541864722391225496 ) ) ;
#5462 = CARTESIAN_POINT ( 'NONE',  ( -1.051607547633159445, 0.4330708661417285721, -1.573502280244651441 ) ) ;
#5463 = ORIENTED_EDGE ( 'NONE', *, *, #4539, .T. ) ;
#5464 = FACE_OUTER_BOUND ( 'NONE', #7391, .T. ) ;
#5465 = B_SPLINE_CURVE_WITH_KNOTS ( 'NONE', 3,
 ( #5481, #275, #916, #4894, #6057, #6119 ),
 .UNSPECIFIED., .F., .F.,
 ( 4, 2, 4 ),
 ( 2.380732026382070147E-07, 0.002190927868076674410, 0.004381617662950710798 ),
 .UNSPECIFIED. ) ;
#5466 = DIRECTION ( 'NONE',  ( 1.000000000000000000, 0.000000000000000000, 0.000000000000000000 ) ) ;
#5467 = CARTESIAN_POINT ( 'NONE',  ( 0.8989365377700750948, -0.4559220466128829363, -1.445239289764781665 ) ) ;
#5468 = CARTESIAN_POINT ( 'NONE',  ( 7.874015748031496287, 0.2559055118110236116, 0.2362204724409455170 ) ) ;
#5469 = CARTESIAN_POINT ( 'NONE',  ( 0.3432736861146661322, -0.1846838951640047688, -0.2706692913385826404 ) ) ;
#5470 = CARTESIAN_POINT ( 'NONE',  ( 0.000000000000000000, 0.000000000000000000, -0.2362204724409449341 ) ) ;
#5471 = CARTESIAN_POINT ( 'NONE',  ( 1.968503937007874072, 1.205361022782827973E-16, -0.9842519685039370358 ) ) ;
#5472 = DIRECTION ( 'NONE',  ( 1.000000000000000000, 0.000000000000000000, 0.000000000000000000 ) ) ;
#5473 = ORIENTED_EDGE ( 'NONE', *, *, #2320, .T. ) ;
#5474 = AXIS2_PLACEMENT_3D ( 'NONE', #288, #4871, #778 ) ;
#5475 = DIRECTION ( 'NONE',  ( 1.000000000000000000, 0.000000000000000000, 0.000000000000000000 ) ) ;
#5476 = EDGE_CURVE ( 'NONE', #7153, #4527, #282, .T. ) ;
#5477 = CARTESIAN_POINT ( 'NONE',  ( 0.2371576072764297882, -0.2722228516542265497, -0.4052515342986934832 ) ) ;
#5478 = EDGE_CURVE ( 'NONE', #6455, #4139, #2238, .T. ) ;
#5479 = EDGE_CURVE ( 'NONE', #1792, #6137, #1638, .T. ) ;
#5480 = ORIENTED_EDGE ( 'NONE', *, *, #3370, .T. ) ;
#5481 = CARTESIAN_POINT ( 'NONE',  ( 0.02637295201093722841, 0.3409548833797004797, 3.882420715168025960E-18 ) ) ;
#5482 = B_SPLINE_CURVE_WITH_KNOTS ( 'NONE', 3,
 ( #3065, #3028, #3492, #5291, #4709, #4181 ),
 .UNSPECIFIED., .F., .F.,
 ( 4, 2, 4 ),
 ( 0.007897041933671775787, 0.01008815886328916570, 0.01227927579290655560 ),
 .UNSPECIFIED. ) ;
#5483 = CARTESIAN_POINT ( 'NONE',  ( 0.3479975484506714345, 0.1192183696110101915, -0.3017044215715822819 ) ) ;
#5484 = CARTESIAN_POINT ( 'NONE',  ( -1.279527559055118280, 1.968503937007874072, 0.4724409448818898127 ) ) ;
#5485 = CARTESIAN_POINT ( 'NONE',  ( 0.9842519685039370358, 0.7480314960629921295, 0.4921259842519685179 ) ) ;
#5486 = ORIENTED_EDGE ( 'NONE', *, *, #4867, .F. ) ;
#5487 = CARTESIAN_POINT ( 'NONE',  ( 0.000000000000000000, 0.000000000000000000, -0.4921259842519685179 ) ) ;
#5488 = AXIS2_PLACEMENT_3D ( 'NONE', #2705, #2743, #1466 ) ;
#5489 = ADVANCED_FACE ( 'NONE', ( #6699 ), #4404, .F. ) ;
#5490 = EDGE_CURVE ( 'NONE', #997, #2864, #2676, .T. ) ;
#5491 = VERTEX_POINT ( 'NONE', #6166 ) ;
#5492 = LINE ( 'NONE', #4253, #3939 ) ;
#5493 = VECTOR ( 'NONE', #1360, 39.37007874015748143 ) ;
#5494 = ORIENTED_EDGE ( 'NONE', *, *, #2578, .F. ) ;
#5495 = CARTESIAN_POINT ( 'NONE',  ( -0.1469816153540868531, -0.3242859848650329058, -2.174273549644897140E-17 ) ) ;
#5496 = EDGE_LOOP ( 'NONE', ( #2690, #2790, #3518, #3153, #2177, #4658 ) ) ;
#5497 = CARTESIAN_POINT ( 'NONE',  ( 0.3391892065151629332, -0.1136516277932338725, -0.2952755905511810774 ) ) ;
#5498 = VERTEX_POINT ( 'NONE', #3792 ) ;
#5499 = CARTESIAN_POINT ( 'NONE',  ( 9.857707340795016185E-18, -0.4091458600556410752, -0.4082677165354330340 ) ) ;
#5500 = AXIS2_PLACEMENT_3D ( 'NONE', #4557, #6890, #6346 ) ;
#5501 = ORIENTED_EDGE ( 'NONE', *, *, #2103, .F. ) ;
#5502 =( NAMED_UNIT ( * ) SI_UNIT ( $, .STERADIAN. ) SOLID_ANGLE_UNIT ( ) );
#5503 = CARTESIAN_POINT ( 'NONE',  ( -0.9659644734970528335, -0.4700904924197936707, -1.546597720061111847 ) ) ;
#5504 = VECTOR ( 'NONE', #5657, 39.37007874015748143 ) ;
#5505 = CARTESIAN_POINT ( 'NONE',  ( 0.4589124540220939630, -1.085572738833920692, -1.540322878613942681 ) ) ;
#5506 = CARTESIAN_POINT ( 'NONE',  ( 1.196439825128248202, 0.1049569639594290504, -0.9787451009560118598 ) ) ;
#5507 = AXIS2_PLACEMENT_3D ( 'NONE', #453, #5039, #4381 ) ;
#5508 = CARTESIAN_POINT ( 'NONE',  ( 1.968503937007874072, 1.496062992125984259, -0.4921259842519685179 ) ) ;
#5509 = CARTESIAN_POINT ( 'NONE',  ( -0.2362204724409449341, 2.892866454678787531E-17, -0.7983802283864780414 ) ) ;
#5510 = DIRECTION ( 'NONE',  ( -0.000000000000000000, -1.000000000000000000, -0.000000000000000000 ) ) ;
#5511 = CYLINDRICAL_SURFACE ( 'NONE', #2175, 0.4921259842519685179 ) ;
#5512 = CARTESIAN_POINT ( 'NONE',  ( -0.1771653543307088186, -0.3068593950417299876, 7.886165872636028972E-17 ) ) ;
#5513 = ORIENTED_EDGE ( 'NONE', *, *, #7418, .F. ) ;
#5514 = DIRECTION ( 'NONE',  ( 0.000000000000000000, 0.000000000000000000, 1.000000000000000000 ) ) ;
#5515 = CARTESIAN_POINT ( 'NONE',  ( 0.000000000000000000, 0.000000000000000000, -1.484898342931014303 ) ) ;
#5516 =( REPRESENTATION_RELATIONSHIP ('NONE','NONE', #303, #1552 ) REPRESENTATION_RELATIONSHIP_WITH_TRANSFORMATION ( #2283 )SHAPE_REPRESENTATION_RELATIONSHIP( ) );
#5517 = EDGE_LOOP ( 'NONE', ( #1295, #5314, #2402, #5916 ) ) ;
#5518 = FACE_OUTER_BOUND ( 'NONE', #1677, .T. ) ;
#5519 = FACE_OUTER_BOUND ( 'NONE', #5517, .T. ) ;
#5520 = PRESENTATION_LAYER_ASSIGNMENT (  '', '', ( #6851 ) ) ;
#5521 = ADVANCED_FACE ( 'NONE', ( #1521 ), #6263, .T. ) ;
#5522 = CARTESIAN_POINT ( 'NONE',  ( 0.4756000659977976941, 1.083679028610379680, -1.522578585053778744 ) ) ;
#5523 = ORIENTED_EDGE ( 'NONE', *, *, #2199, .F. ) ;
#5524 = CARTESIAN_POINT ( 'NONE',  ( 0.4541662050560835162, -0.9857970000181582870, -1.560880783937514504 ) ) ;
#5525 = CIRCLE ( 'NONE', #6488, 0.3543307086614173596 ) ;
#5526 = EDGE_LOOP ( 'NONE', ( #2903, #3529, #5012, #3782, #5691, #1379, #2612 ) ) ;
#5527 = PRODUCT_DEFINITION_SHAPE ( 'NONE', 'NONE',  #7527 ) ;
#5528 = B_SPLINE_CURVE_WITH_KNOTS ( 'NONE', 3,
 ( #5085, #7402, #3937, #5126, #6563, #180, #1180, #7011, #1761, #3530 ),
 .UNSPECIFIED., .F., .F.,
 ( 4, 2, 2, 2, 4 ),
 ( -7.765797721848017974E-06, 0.0005114169989440522576, 0.001030599795609952584, 0.001549782592275852910, 0.002068965388941753237 ),
 .UNSPECIFIED. ) ;
#5529 = ORIENTED_EDGE ( 'NONE', *, *, #6316, .F. ) ;
#5530 = DIRECTION ( 'NONE',  ( 0.000000000000000000, 1.000000000000000000, -1.001543065824774208E-16 ) ) ;
#5531 = SHAPE_REPRESENTATION ( 'Supporter 2', ( #5166 ), #4173 ) ;
#5532 = EDGE_CURVE ( 'NONE', #1492, #383, #6150, .T. ) ;
#5533 = DIRECTION ( 'NONE',  ( 0.000000000000000000, 1.000000000000000000, 0.000000000000000000 ) ) ;
#5534 = VERTEX_POINT ( 'NONE', #3214 ) ;
#5535 = EDGE_CURVE ( 'NONE', #4759, #4696, #6846, .T. ) ;
#5536 = CARTESIAN_POINT ( 'NONE',  ( 0.3337354549120238878, 0.2853048623713461129, 0.09638866382874489158 ) ) ;
#5537 = ORIENTED_EDGE ( 'NONE', *, *, #3231, .T. ) ;
#5538 = AXIS2_PLACEMENT_3D ( 'NONE', #1262, #4747, #7080 ) ;
#5539 = CARTESIAN_POINT ( 'NONE',  ( 0.7723175066527832033, 0.1046133869837157365, 0.9787008116518934875 ) ) ;
#5540 = ORIENTED_EDGE ( 'NONE', *, *, #5762, .F. ) ;
#5541 = CARTESIAN_POINT ( 'NONE',  ( 0.000000000000000000, 1.496062992125984259, -0.4921259842519685179 ) ) ;
#5542 = EDGE_CURVE ( 'NONE', #1972, #630, #4185, .T. ) ;
#5543 = TOROIDAL_SURFACE ( 'NONE', #1368, 1.124634398195722973, 0.05905511811023622659 ) ;
#5544 = EDGE_LOOP ( 'NONE', ( #6893, #6051, #1164, #5034 ) ) ;
#5545 = DIRECTION ( 'NONE',  ( 1.000000000000000000, 0.000000000000000000, -0.000000000000000000 ) ) ;
#5546 = AXIS2_PLACEMENT_3D ( 'NONE', #4558, #4481, #2753 ) ;
#5547 = CARTESIAN_POINT ( 'NONE',  ( 0.4348450093584661502, -1.063161251382698680, -1.569784523562343770 ) ) ;
#5548 = AXIS2_PLACEMENT_3D ( 'NONE', #600, #5807, #6375 ) ;
#5549 = CARTESIAN_POINT ( 'NONE',  ( -2.834645669291338432, 0.4724409448818890911, 0.4724409448818902013 ) ) ;
#5550 = CARTESIAN_POINT ( 'NONE',  ( 0.01832242175888482497, -0.3270109559553083245, 0.02415159075610082487 ) ) ;
#5551 = CARTESIAN_POINT ( 'NONE',  ( 0.9659644734970590507, -0.4700904924197804591, -1.546597720061111847 ) ) ;
#5552 = CARTESIAN_POINT ( 'NONE',  ( 0.7480314960629922405, 1.220472440944881942, 2.480314960629921295 ) ) ;
#5553 = ORIENTED_EDGE ( 'NONE', *, *, #3644, .F. ) ;
#5554 = CARTESIAN_POINT ( 'NONE',  ( 0.4330708661417324024, 0.000000000000000000, 0.000000000000000000 ) ) ;
#5555 = CARTESIAN_POINT ( 'NONE',  ( -0.4332776171645011942, 1.054581729003112756, -1.572814845875644574 ) ) ;
#5556 = ORIENTED_EDGE ( 'NONE', *, *, #6089, .F. ) ;
#5557 = CARTESIAN_POINT ( 'NONE',  ( 0.02637295201093703412, 0.1704774416898499345, 0.2952755905511810774 ) ) ;
#5558 = CARTESIAN_POINT ( 'NONE',  ( 0.3565325281581928074, 0.1767208741530144900, -0.2952755905511811330 ) ) ;
#5559 = TOROIDAL_SURFACE ( 'NONE', #1640, 1.223643328182682621, 0.05905511811023622659 ) ;
#5560 = DIRECTION ( 'NONE',  ( 3.491481338843133750E-15, -1.000000000000000000, -4.625929269271482167E-15 ) ) ;
#5561 = ORIENTED_EDGE ( 'NONE', *, *, #7472, .F. ) ;
#5562 = CARTESIAN_POINT ( 'NONE',  ( 0.3483227611829846637, -0.1704774416898499345, 0.2952755905511811330 ) ) ;
#5563 = ORIENTED_EDGE ( 'NONE', *, *, #5109, .T. ) ;
#5564 = ADVANCED_FACE ( 'NONE', ( #4285 ), #2335, .F. ) ;
#5565 = VERTEX_POINT ( 'NONE', #999 ) ;
#5566 = DIRECTION ( 'NONE',  ( 0.000000000000000000, 0.000000000000000000, -1.000000000000000000 ) ) ;
#5567 = CARTESIAN_POINT ( 'NONE',  ( 0.9984400756355412687, 0.4637694296357287582, -1.410742812766315746 ) ) ;
#5568 = CARTESIAN_POINT ( 'NONE',  ( 0.3574269917172687161, -0.3465569331832414335, -9.402262055513304185E-15 ) ) ;
#5569 = CARTESIAN_POINT ( 'NONE',  ( 0.7480314960629922405, 0.7480314960629921295, 0.000000000000000000 ) ) ;
#5570 = EDGE_LOOP ( 'NONE', ( #1852, #5782, #2494, #3108 ) ) ;
#5571 = CARTESIAN_POINT ( 'NONE',  ( 0.3527008206095850751, 0.3418447298186451655, 4.692841048826145323E-17 ) ) ;
#5572 = FACE_OUTER_BOUND ( 'NONE', #2717, .T. ) ;
#5573 = ADVANCED_FACE ( 'NONE', ( #3443 ), #1645, .F. ) ;
#5574 = ORIENTED_EDGE ( 'NONE', *, *, #3427, .T. ) ;
#5575 = ADVANCED_FACE ( 'NONE', ( #3407 ), #7448, .F. ) ;
#5576 = VERTEX_POINT ( 'NONE', #2146 ) ;
#5577 = EDGE_CURVE ( 'NONE', #1208, #1565, #4064, .T. ) ;
#5578 = CARTESIAN_POINT ( 'NONE',  ( 25.35842062421581389, 45.20863634146751764, 51.90956403617311565 ) ) ;
#5579 = CARTESIAN_POINT ( 'NONE',  ( -0.5141614760841463072, 0.9609181420092333115, -1.361499588670821659 ) ) ;
#5580 = EDGE_CURVE ( 'NONE', #5905, #1170, #3290, .T. ) ;
#5581 = CARTESIAN_POINT ( 'NONE',  ( 0.003035684155427062578, 0.2268414356900468054, -0.1976502892253328703 ) ) ;
#5582 = CARTESIAN_POINT ( 'NONE',  ( 1.128157436560226712, -0.1874853199515785218, -0.9662432197917761867 ) ) ;
#5583 = B_SPLINE_CURVE_WITH_KNOTS ( 'NONE', 3,
 ( #77, #4126, #2559, #2403, #6461, #121 ),
 .UNSPECIFIED., .F., .F.,
 ( 4, 2, 4 ),
 ( 0.000000000000000000, 0.002233368740102886427, 0.004466737480205772853 ),
 .UNSPECIFIED. ) ;
#5584 = CARTESIAN_POINT ( 'NONE',  ( 0.000000000000000000, -0.2557161625347748601, 0.1476377952755911216 ) ) ;
#5585 = ADVANCED_FACE ( 'NONE', ( #6279 ), #3215, .F. ) ;
#5586 = DIRECTION ( 'NONE',  ( 0.000000000000000000, 0.000000000000000000, -1.000000000000000000 ) ) ;
#5587 = LINE ( 'NONE', #5083, #6632 ) ;
#5588 = CARTESIAN_POINT ( 'NONE',  ( 0.3510872220068100846, -0.1819230426404178091, 0.2754512281816298147 ) ) ;
#5589 = CARTESIAN_POINT ( 'NONE',  ( 1.037563309807729262, -0.4338950423154036007, -1.574803149606299302 ) ) ;
#5590 = VERTEX_POINT ( 'NONE', #545 ) ;
#5591 = PRODUCT ( 'Link', 'Link', '', ( #777 ) ) ;
#5592 = DIRECTION ( 'NONE',  ( 0.000000000000000000, 0.000000000000000000, -1.000000000000000000 ) ) ;
#5593 = ORIENTED_EDGE ( 'NONE', *, *, #1033, .F. ) ;
#5594 = SPHERICAL_SURFACE ( 'NONE', #1886, 1.377952755905511806 ) ;
#5595 = CARTESIAN_POINT ( 'NONE',  ( 0.3409815385080205985, -0.02878389060673587282, -0.3014914578570770387 ) ) ;
#5596 = PRODUCT_CONTEXT ( 'NONE', #3255, 'mechanical' ) ;
#5597 = DIRECTION ( 'NONE',  ( -0.000000000000000000, 0.000000000000000000, 1.000000000000000000 ) ) ;
#5598 = ORIENTED_EDGE ( 'NONE', *, *, #7245, .F. ) ;
#5599 = DIRECTION ( 'NONE',  ( 1.047444401652940007E-14, -1.000000000000000000, 0.000000000000000000 ) ) ;
#5600 = VERTEX_POINT ( 'NONE', #6314 ) ;
#5601 = AXIS2_PLACEMENT_3D ( 'NONE', #1881, #2935, #4090 ) ;
#5602 = ORIENTED_EDGE ( 'NONE', *, *, #2255, .T. ) ;
#5603 = PLANE ( 'NONE',  #6623 ) ;
#5604 = CARTESIAN_POINT ( 'NONE',  ( 0.3485373078438442351, 0.3194486952732363827, 0.05009812457233156491 ) ) ;
#5605 = CARTESIAN_POINT ( 'NONE',  ( -1.279527559055118280, 1.968503937007874072, 0.000000000000000000 ) ) ;
#5606 = EDGE_LOOP ( 'NONE', ( #5442, #3454, #3510, #7377 ) ) ;
#5607 = CARTESIAN_POINT ( 'NONE',  ( 0.4700904924197906176, -0.9659644734970541657, -1.546597720061111847 ) ) ;
#5608 = ORIENTED_EDGE ( 'NONE', *, *, #1349, .F. ) ;
#5609 = CONICAL_SURFACE ( 'NONE', #6695, 0.3543307086614173596, 1.047197551196596521 ) ;
#5610 = CARTESIAN_POINT ( 'NONE',  ( 7.874015748031496287, 0.2559055118110236116, -0.4921259842519685179 ) ) ;
#5611 = VERTEX_POINT ( 'NONE', #1066 ) ;
#5612 = FACE_OUTER_BOUND ( 'NONE', #3205, .T. ) ;
#5613 = EDGE_LOOP ( 'NONE', ( #5602, #6514, #5320 ) ) ;
#5614 = VERTEX_POINT ( 'NONE', #5749 ) ;
#5615 = CARTESIAN_POINT ( 'NONE',  ( 0.002549129251883240199, 0.05807386165065146072, -0.2952755905511810219 ) ) ;
#5616 = VECTOR ( 'NONE', #5970, 39.37007874015748143 ) ;
#5617 = DIRECTION ( 'NONE',  ( 0.4186275392765895775, -0.9081580167345476573, 1.638878670390340615E-16 ) ) ;
#5618 = CARTESIAN_POINT ( 'NONE',  ( 0.000000000000000000, 1.496062992125984259, 0.000000000000000000 ) ) ;
#5619 = CARTESIAN_POINT ( 'NONE',  ( 0.000000000000000000, 0.000000000000000000, 0.000000000000000000 ) ) ;
#5620 = CARTESIAN_POINT ( 'NONE',  ( 1.208238579388023037, -0.07659700195593643901, -0.9813707449069869471 ) ) ;
#5621 = APPLICATION_CONTEXT ( 'automotive_design' ) ;
#5622 = EDGE_CURVE ( 'NONE', #4413, #2064, #1618, .T. ) ;
#5623 = AXIS2_PLACEMENT_3D ( 'NONE', #2484, #158, #3123 ) ;
#5624 = CARTESIAN_POINT ( 'NONE',  ( 0.4921259842519683514, 0.000000000000000000, -2.204724409448820754 ) ) ;
#5625 = CARTESIAN_POINT ( 'NONE',  ( 0.9688787811271879491, 0.2362268424322147564, -0.9554835511204313736 ) ) ;
#5626 = AXIS2_PLACEMENT_3D ( 'NONE', #560, #4578, #6438 ) ;
#5627 = CARTESIAN_POINT ( 'NONE',  ( 0.1771653543307088463, 0.3068593950417300431, 7.886165872636028972E-17 ) ) ;
#5628 = ADVANCED_FACE ( 'NONE', ( #2289 ), #6956, .F. ) ;
#5629 = DIRECTION ( 'NONE',  ( -1.000000000000000000, 0.000000000000000000, 0.000000000000000000 ) ) ;
#5630 = DIRECTION ( 'NONE',  ( 0.000000000000000000, 0.000000000000000000, 1.000000000000000000 ) ) ;
#5631 = ADVANCED_FACE ( 'NONE', ( #1097, #6201, #1162 ), #3550, .T. ) ;
#5632 = VERTEX_POINT ( 'NONE', #610 ) ;
#5633 = CARTESIAN_POINT ( 'NONE',  ( 0.3483227611829846637, 0.1704774416898499345, 0.2952755905511810774 ) ) ;
#5634 = AXIS2_PLACEMENT_3D ( 'NONE', #713, #2999, #5379 ) ;
#5635 = EDGE_CURVE ( 'NONE', #4456, #6362, #4051, .T. ) ;
#5636 = ORIENTED_EDGE ( 'NONE', *, *, #340, .F. ) ;
#5637 = CARTESIAN_POINT ( 'NONE',  ( 0.3574269917172681610, 0.1732784665916975442, -0.3001271079942677833 ) ) ;
#5638 = CARTESIAN_POINT ( 'NONE',  ( 0.3581828924050323715, -0.1743168766271109560, 0.3019256869348722616 ) ) ;
#5639 = DIRECTION ( 'NONE',  ( 0.8660254037844382635, -0.5000000000000005551, 0.000000000000000000 ) ) ;
#5640 = ORIENTED_EDGE ( 'NONE', *, *, #7151, .T. ) ;
#5641 = LINE ( 'NONE', #6954, #493 ) ;
#5642 = ORIENTED_EDGE ( 'NONE', *, *, #1974, .T. ) ;
#5643 = CIRCLE ( 'NONE', #1836, 1.124634398195722973 ) ;
#5644 = ORIENTED_EDGE ( 'NONE', *, *, #5003, .T. ) ;
#5645 = CARTESIAN_POINT ( 'NONE',  ( 0.3432736861146659657, 0.1420645347415414039, -0.2952755905511810219 ) ) ;
#5646 = EDGE_LOOP ( 'NONE', ( #1454, #6350, #127, #4359 ) ) ;
#5647 = DIRECTION ( 'NONE',  ( -0.000000000000000000, -0.000000000000000000, 1.000000000000000000 ) ) ;
#5648 = VERTEX_POINT ( 'NONE', #3012 ) ;
#5649 = AXIS2_PLACEMENT_3D ( 'NONE', #430, #1555, #1673 ) ;
#5650 = CARTESIAN_POINT ( 'NONE',  ( 1.102581283201567564, 0.2050316615124324060, 0.9626998336838916703 ) ) ;
#5651 = ORIENTED_EDGE ( 'NONE', *, *, #2978, .T. ) ;
#5652 = ORIENTED_EDGE ( 'NONE', *, *, #1825, .F. ) ;
#5653 = ORIENTED_EDGE ( 'NONE', *, *, #1975, .T. ) ;
#5654 = DIRECTION ( 'NONE',  ( -1.000000000000000000, -0.000000000000000000, -4.625929269271482167E-15 ) ) ;
#5655 = DIRECTION ( 'NONE',  ( -0.9081580167345477683, -0.4186275392765896330, -3.538501663742126977E-16 ) ) ;
#5656 = CIRCLE ( 'NONE', #2332, 0.2362204724409449341 ) ;
#5657 = DIRECTION ( 'NONE',  ( -0.000000000000000000, -0.000000000000000000, 1.000000000000000000 ) ) ;
#5658 = FACE_OUTER_BOUND ( 'NONE', #3554, .T. ) ;
#5659 = SURFACE_STYLE_FILL_AREA ( #3310 ) ;
#5660 = AXIS2_PLACEMENT_3D ( 'NONE', #5318, #171, #5980 ) ;
#5661 = PLANE ( 'NONE',  #3336 ) ;
#5662 = PRODUCT_DEFINITION ( 'UNKNOWN', '', #935, #754 ) ;
#5663 = CARTESIAN_POINT ( 'NONE',  ( 0.4659838021912668382, 0.9705345056684758775, -1.550372027848113010 ) ) ;
#5664 = VECTOR ( 'NONE', #4827, 39.37007874015748143 ) ;
#5665 = CARTESIAN_POINT ( 'NONE',  ( 0.3432736861146661322, 0.3267484299055462005, -0.02460629921259842659 ) ) ;
#5666 = CIRCLE ( 'NONE', #6754, 1.074277634097407175 ) ;
#5667 = CARTESIAN_POINT ( 'NONE',  ( 0.5118110236220474452, 1.220472440944881942, 2.952755905511811108 ) ) ;
#5668 = CARTESIAN_POINT ( 'NONE',  ( 0.000000000000000000, 0.000000000000000000, -2.204724409448820754 ) ) ;
#5669 = CARTESIAN_POINT ( 'NONE',  ( 8.136851934253910637E-18, -0.02882762270234999827, 0.2952755905511811330 ) ) ;
#5670 = AXIS2_PLACEMENT_3D ( 'NONE', #7141, #3672, #6011 ) ;
#5671 = CARTESIAN_POINT ( 'NONE',  ( 0.4330708661417321803, -0.9697097640641195726, -1.453662949853142594 ) ) ;
#5672 = EDGE_CURVE ( 'NONE', #135, #6850, #6474, .T. ) ;
#5673 = EDGE_CURVE ( 'NONE', #5757, #5718, #4655, .T. ) ;
#5674 = PLANE ( 'NONE',  #5649 ) ;
#5675 = B_SPLINE_CURVE_WITH_KNOTS ( 'NONE', 3,
 ( #6613, #1322, #3668, #3165, #1398, #3743, #4274, #6007 ),
 .UNSPECIFIED., .F., .F.,
 ( 4, 2, 2, 4 ),
 ( 0.005257893453559907976, 0.006567392922673238181, 0.007876892391786568387, 0.01049589133001323227 ),
 .UNSPECIFIED. ) ;
#5676 = EDGE_CURVE ( 'NONE', #4304, #733, #2015, .T. ) ;
#5677 = CARTESIAN_POINT ( 'NONE',  ( -0.9960023578760569540, -0.4720886891211169001, -1.401719942879701364 ) ) ;
#5678 = EDGE_LOOP ( 'NONE', ( #3418, #3922, #7187, #1161 ) ) ;
#5679 = CARTESIAN_POINT ( 'NONE',  ( 0.3322361761492158561, -0.2866471735583170366, 0.09406371265334383114 ) ) ;
#5680 = B_SPLINE_CURVE_WITH_KNOTS ( 'NONE', 3,
 ( #3473, #991, #2164, #4044, #7510, #6309, #3944, #1598, #5200, #4616 ),
 .UNSPECIFIED., .F., .F.,
 ( 4, 2, 2, 2, 4 ),
 ( 0.000000000000000000, 0.0005216184974661242351, 0.001043236994932248470, 0.001564855492398372705, 0.002086473989864496940 ),
 .UNSPECIFIED. ) ;
#5681 = ORIENTED_EDGE ( 'NONE', *, *, #3887, .T. ) ;
#5682 = ORIENTED_EDGE ( 'NONE', *, *, #7340, .F. ) ;
#5683 = B_SPLINE_CURVE_WITH_KNOTS ( 'NONE', 3,
 ( #7444, #2713, #6915, #4514, #7407, #7482, #5709, #541 ),
 .UNSPECIFIED., .F., .F.,
 ( 4, 2, 2, 4 ),
 ( 0.005257893453559898435, 0.006567392922673230375, 0.007876892391786563183, 0.01049589133001322706 ),
 .UNSPECIFIED. ) ;
#5684 = EDGE_CURVE ( 'NONE', #4791, #4898, #4779, .T. ) ;
#5685 = TOROIDAL_SURFACE ( 'NONE', #3472, 0.2952755905511811885, 0.05905511811023622659 ) ;
#5686 = LINE ( 'NONE', #2725, #1721 ) ;
#5687 = DIRECTION ( 'NONE',  ( -2.207829878515936732E-15, 0.000000000000000000, 1.000000000000000000 ) ) ;
#5688 =( LENGTH_UNIT ( ) NAMED_UNIT ( * ) SI_UNIT ( $, .METRE. ) );
#5689 = ORIENTED_EDGE ( 'NONE', *, *, #5432, .T. ) ;
#5690 = CARTESIAN_POINT ( 'NONE',  ( 0.3432736861146661878, -0.3267484299055466446, 0.02460629921259842312 ) ) ;
#5691 = ORIENTED_EDGE ( 'NONE', *, *, #6556, .F. ) ;
#5692 = CARTESIAN_POINT ( 'NONE',  ( -0.2073036836782042036, -0.2894590224800286937, -0.4075196867561204361 ) ) ;
#5693 = CIRCLE ( 'NONE', #3352, 0.2699662542182227343 ) ;
#5694=STYLED_ITEM('',(#7587),#1558);
#5695 = CARTESIAN_POINT ( 'NONE',  ( 0.3581828924050323715, -0.1743168766271109560, 0.3019256869348722616 ) ) ;
#5696 = ORIENTED_EDGE ( 'NONE', *, *, #1919, .F. ) ;
#5697 = DIRECTION ( 'NONE',  ( -0.000000000000000000, -0.000000000000000000, -1.000000000000000000 ) ) ;
#5698 = CARTESIAN_POINT ( 'NONE',  ( 33.89456220083551585, 40.86510553865259254, 51.90956403617311565 ) ) ;
#5699 = DIRECTION ( 'NONE',  ( -1.000000000000000000, -0.000000000000000000, -0.000000000000000000 ) ) ;
#5700 = CARTESIAN_POINT ( 'NONE',  ( 0.9609181420092369752, -0.5141614760841358711, -1.361499588670819216 ) ) ;
#5701 = B_SPLINE_CURVE_WITH_KNOTS ( 'NONE', 3,
 ( #341, #2095, #3084, #4964 ),
 .UNSPECIFIED., .F., .F.,
 ( 4, 4 ),
 ( 0.000000000000000000, 0.0002807012396509386419 ),
 .UNSPECIFIED. ) ;
#5702 = DIRECTION ( 'NONE',  ( 0.000000000000000000, 0.000000000000000000, -1.000000000000000000 ) ) ;
#5703 = CARTESIAN_POINT ( 'NONE',  ( 0.8658672433185115036, 0.2045602151624222043, -0.9627673662903735163 ) ) ;
#5704 = CARTESIAN_POINT ( 'NONE',  ( 0.4685039370078740717, 0.1704774416898497680, -0.2952755905511810774 ) ) ;
#5705 = CARTESIAN_POINT ( 'NONE',  ( 7.874015748031496287, 0.2559055118110236116, 0.000000000000000000 ) ) ;
#5706 = LINE ( 'NONE', #7478, #5770 ) ;
#5707 = VERTEX_POINT ( 'NONE', #4205 ) ;
#5708 = CARTESIAN_POINT ( 'NONE',  ( 6.221505307624544299E-30, -1.781909941321919274E-15, -1.397637795275591843 ) ) ;
#5709 = CARTESIAN_POINT ( 'NONE',  ( 0.3254211578371891678, 0.2212638669783393297, -0.3862566910637258433 ) ) ;
#5710 = CARTESIAN_POINT ( 'NONE',  ( 0.3483227611829849413, -0.3409548833797009237, 0.000000000000000000 ) ) ;
#5711 = ORIENTED_EDGE ( 'NONE', *, *, #2479, .T. ) ;
#5713 = CARTESIAN_POINT ( 'NONE',  ( 1.054581729003116530, -0.4332776171644905916, -1.572814845875644352 ) ) ;
#5712 = DIMENSIONAL_EXPONENTS ( 1.000000000000000000, 0.000000000000000000, 0.000000000000000000, 0.000000000000000000, 0.000000000000000000, 0.000000000000000000, 0.000000000000000000 ) ;
#5714 = AXIS2_PLACEMENT_3D ( 'NONE', #3425, #4137, #4068 ) ;
#5715 = CARTESIAN_POINT ( 'NONE',  ( 0.000000000000000000, 0.000000000000000000, -0.4082677165354330340 ) ) ;
#5716 = ADVANCED_FACE ( 'NONE', ( #5271 ), #6512, .T. ) ;
#5717 = ORIENTED_EDGE ( 'NONE', *, *, #4539, .F. ) ;
#5718 = VERTEX_POINT ( 'NONE', #651 ) ;
#5719 = CARTESIAN_POINT ( 'NONE',  ( -0.2371576072764296494, 0.2722228516542259946, -0.003016182236739215101 ) ) ;
#5720 = VERTEX_POINT ( 'NONE', #3629 ) ;
#5721 = DIRECTION ( 'NONE',  ( 0.000000000000000000, 0.000000000000000000, -1.000000000000000000 ) ) ;
#5722 = ORIENTED_EDGE ( 'NONE', *, *, #3321, .F. ) ;
#5723 = CARTESIAN_POINT ( 'NONE',  ( 0.9604263920613147487, 0.4330708661417422833, -1.456063616177416087 ) ) ;
#5724 = ADVANCED_FACE ( 'NONE', ( #4694 ), #1244, .F. ) ;
#5725 = ADVANCED_FACE ( 'NONE', ( #5397 ), #2488, .F. ) ;
#5726 =( GEOMETRIC_REPRESENTATION_CONTEXT ( 3 ) GLOBAL_UNCERTAINTY_ASSIGNED_CONTEXT ( ( #6337 ) ) GLOBAL_UNIT_ASSIGNED_CONTEXT ( ( #4455, #251, #6855 ) ) REPRESENTATION_CONTEXT ( 'NONE', 'WORKASPACE' ) );
#5727 = ORIENTED_EDGE ( 'NONE', *, *, #7058, .F. ) ;
#5728 = FACE_OUTER_BOUND ( 'NONE', #3409, .T. ) ;
#5729 = CARTESIAN_POINT ( 'NONE',  ( 26.63278072698489041, 34.81515369617522992, 55.32688687081880374 ) ) ;
#5730 = LINE ( 'NONE', #5154, #7222 ) ;
#5731 = CARTESIAN_POINT ( 'NONE',  ( 0.4685039370078740717, 0.000000000000000000, 0.000000000000000000 ) ) ;
#5732 = SURFACE_STYLE_USAGE ( .BOTH. , #4034 ) ;
#5733 = CARTESIAN_POINT ( 'NONE',  ( 0.01171324505787554697, -0.1984117137466534231, 0.2468920120763462012 ) ) ;
#5734 = CARTESIAN_POINT ( 'NONE',  ( 0.8284312913633176123, 0.1777059077220142780, -0.9680895064399986927 ) ) ;
#5735 = TOROIDAL_SURFACE ( 'NONE', #3275, 1.223643328182681289, 0.05905511811023622659 ) ;
#5736 =( NAMED_UNIT ( * ) SI_UNIT ( $, .STERADIAN. ) SOLID_ANGLE_UNIT ( ) );
#5737 = CARTESIAN_POINT ( 'NONE',  ( 0.000000000000000000, 1.496062992125984259, -0.2362204724409449341 ) ) ;
#5738 = VECTOR ( 'NONE', #5436, 39.37007874015748143 ) ;
#5739 = DIRECTION ( 'NONE',  ( -0.8191520442889907994, 0.000000000000000000, -0.5735764363510474917 ) ) ;
#5740 = CARTESIAN_POINT ( 'NONE',  ( 0.000000000000000000, 0.000000000000000000, 0.1188976377952756375 ) ) ;
#5741 = FACE_OUTER_BOUND ( 'NONE', #2297, .T. ) ;
#5742 = VECTOR ( 'NONE', #4882, 39.37007874015748143 ) ;
#5743 = FACE_OUTER_BOUND ( 'NONE', #3795, .T. ) ;
#5744 = DIRECTION ( 'NONE',  ( -2.312579046053608732E-29, 2.207829878515936732E-15, 1.000000000000000000 ) ) ;
#5745 = PLANE ( 'NONE',  #4250 ) ;
#5746 = ORIENTED_EDGE ( 'NONE', *, *, #1078, .T. ) ;
#5747 = FACE_OUTER_BOUND ( 'NONE', #6312, .T. ) ;
#5748 = CIRCLE ( 'NONE', #861, 0.2362204724409449341 ) ;
#5749 = CARTESIAN_POINT ( 'NONE',  ( -0.2362204724409449619, 2.892866454678788147E-17, -0.4082677165354330340 ) ) ;
#5750 = ORIENTED_EDGE ( 'NONE', *, *, #2059, .F. ) ;
#5751 = CARTESIAN_POINT ( 'NONE',  ( 1.067758866085110281, -0.2211013871911202966, 0.9591012775692122627 ) ) ;
#5752 = AXIS2_PLACEMENT_3D ( 'NONE', #4675, #667, #4099 ) ;
#5753 = EDGE_CURVE ( 'NONE', #6423, #6850, #3825, .T. ) ;
#5754 = CARTESIAN_POINT ( 'NONE',  ( 0.3336175750056032951, -0.05682581389661717219, -0.2952755905511811330 ) ) ;
#5755 = ORIENTED_EDGE ( 'NONE', *, *, #2013, .F. ) ;
#5756 = CARTESIAN_POINT ( 'NONE',  ( 0.3585665126877356501, 0.3496831043983829046, -0.001800812819183686539 ) ) ;
#5757 = VERTEX_POINT ( 'NONE', #1205 ) ;
#5758 = ORIENTED_EDGE ( 'NONE', *, *, #943, .T. ) ;
#5759 = DIMENSIONAL_EXPONENTS ( 1.000000000000000000, 0.000000000000000000, 0.000000000000000000, 0.000000000000000000, 0.000000000000000000, 0.000000000000000000, 0.000000000000000000 ) ;
#5760 = FACE_BOUND ( 'NONE', #6640, .T. ) ;
#5761 = EDGE_CURVE ( 'NONE', #4433, #1688, #3572, .T. ) ;
#5762 = EDGE_CURVE ( 'NONE', #139, #1597, #7288, .T. ) ;
#5763 = CIRCLE ( 'NONE', #3801, 0.4921259842519685179 ) ;
#5764 = B_SPLINE_CURVE_WITH_KNOTS ( 'NONE', 3,
 ( #2174, #6156, #7323, #4508, #6841, #912, #1593, #1022 ),
 .UNSPECIFIED., .F., .F.,
 ( 4, 2, 2, 4 ),
 ( 0.004381617662950689981, 0.005472867551409524994, 0.006564117439868360007, 0.008746617216786028298 ),
 .UNSPECIFIED. ) ;
#5765 = CARTESIAN_POINT ( 'NONE',  ( 0.3574269917172687161, -0.3465569331832414335, -9.402262055513304185E-15 ) ) ;
#5766 = PRESENTATION_STYLE_ASSIGNMENT (( #2877 ) ) ;
#5767 = B_SPLINE_CURVE_WITH_KNOTS ( 'NONE', 3,
 ( #4151, #4114, #681, #2920, #3541, #717 ),
 .UNSPECIFIED., .F., .F.,
 ( 4, 2, 4 ),
 ( 2.380730968541169696E-07, 0.002629065763328381714, 0.005257893453559908843 ),
 .UNSPECIFIED. ) ;
#5768 = DIRECTION ( 'NONE',  ( 0.000000000000000000, 0.000000000000000000, -1.000000000000000000 ) ) ;
#5769 =( BOUNDED_SURFACE ( )  B_SPLINE_SURFACE ( 3, 2, ( 
 ( #2684, #3107, #5026 ),
 ( #2571, #3729, #6634 ),
 ( #6136, #5454, #2123 ),
 ( #1965, #216, #857 ),
 ( #5536, #4872, #4457 ),
 ( #7234, #1528, #4294 ),
 ( #2007, #6026, #779 ),
 ( #4338, #7194, #5756 ) ),
 .UNSPECIFIED., .F., .F., .F. ) 
 B_SPLINE_SURFACE_WITH_KNOTS ( ( 4, 2, 2, 4 ),
 ( 3, 3 ),
 ( 0.03551798592901333346, 0.03994769179990642627, 0.04216254473535296921, 0.04437739767079951908 ),
 ( 0.000000000000000000, 1.000000000000000000 ),
 .UNSPECIFIED. ) 
 GEOMETRIC_REPRESENTATION_ITEM ( )  RATIONAL_B_SPLINE_SURFACE ( (
 ( 1.000000000000000000, 0.8047781103519391355, 1.000000000000000000),
 ( 1.000000000000000000, 0.8123785826169017676, 1.000000000000000000),
 ( 1.000000000000000000, 0.8190671539036440407, 1.000000000000000000),
 ( 1.000000000000000000, 0.8191932076449144340, 1.000000000000000000),
 ( 1.000000000000000000, 0.8176085094066379844, 1.000000000000000000),
 ( 1.000000000000000000, 0.8122955484014008354, 1.000000000000000000),
 ( 1.000000000000000000, 0.8086308001280846369, 1.000000000000000000),
 ( 1.000000000000000000, 0.8047712537969720081, 1.000000000000000000) ) ) 
 REPRESENTATION_ITEM ( '' )  SURFACE ( )  );
#5770 = VECTOR ( 'NONE', #6802, 39.37007874015748143 ) ;
#5771 = DIRECTION ( 'NONE',  ( -1.000000000000000000, -0.000000000000000000, -0.000000000000000000 ) ) ;
#5772 = AXIS2_PLACEMENT_3D ( 'NONE', #3966, #1658, #1538 ) ;
#5773 = SPHERICAL_SURFACE ( 'NONE', #2587, 1.259842519685039131 ) ;
#5774 = AXIS2_PLACEMENT_3D ( 'NONE', #5863, #3458, #3424 ) ;
#5775 = PLANE ( 'NONE',  #1243 ) ;
#5776 = CONICAL_SURFACE ( 'NONE', #4302, 0.2952755905511810774, 1.047197551196600518 ) ;
#5777 = CARTESIAN_POINT ( 'NONE',  ( -0.05806029764938282212, 0.3756247315785394836, -0.01405589313879331177 ) ) ;
#5778 = DIRECTION ( 'NONE',  ( 0.000000000000000000, 0.000000000000000000, 1.000000000000000000 ) ) ;
#5779 = B_SPLINE_CURVE_WITH_KNOTS ( 'NONE', 3,
 ( #323, #2726, #2230, #4523 ),
 .UNSPECIFIED., .F., .F.,
 ( 4, 4 ),
 ( 0.000000000000000000, 0.0004815725036528541126 ),
 .UNSPECIFIED. ) ;
#5780 = ITEM_DEFINED_TRANSFORMATION ( 'NONE', 'NONE', #20,  #5166 ) ;
#5781 = DIRECTION ( 'NONE',  ( -1.000000000000000000, 0.000000000000000000, 0.000000000000000000 ) ) ;
#5782 = ORIENTED_EDGE ( 'NONE', *, *, #1924, .F. ) ;
#5783 = CARTESIAN_POINT ( 'NONE',  ( 0.3398312250857988270, 0.1962691648278992451, -0.2506030156613296422 ) ) ;
#5784 = CARTESIAN_POINT ( 'NONE',  ( 0.3391216574608478806, -0.3159523085418498023, 0.04330572993920116937 ) ) ;
#5785 = ORIENTED_EDGE ( 'NONE', *, *, #5432, .F. ) ;
#5786 = ORIENTED_EDGE ( 'NONE', *, *, #4259, .T. ) ;
#5787 = CIRCLE ( 'NONE', #4785, 1.168853328413308690 ) ;
#5788 = CARTESIAN_POINT ( 'NONE',  ( 1.218928898036171882, -0.03106543388645563800, 0.9838782854499440456 ) ) ;
#5789 = VERTEX_POINT ( 'NONE', #312 ) ;
#5790 = DIRECTION ( 'NONE',  ( 1.000000000000000000, 0.000000000000000000, 0.000000000000000000 ) ) ;
#5791 = EDGE_CURVE ( 'NONE', #7462, #345, #5312, .T. ) ;
#5792 = CARTESIAN_POINT ( 'NONE',  ( 0.3426147637089221321, -0.05832033309504448121, 0.3015404986019939448 ) ) ;
#5793 = EDGE_LOOP ( 'NONE', ( #5063, #3421, #1910, #5861 ) ) ;
#5794 = AXIS2_PLACEMENT_3D ( 'NONE', #4926, #2025, #6719 ) ;
#5795=STYLED_ITEM('',(#7587),#1545);
#5796 = DIRECTION ( 'NONE',  ( -1.000000000000000000, -0.000000000000000000, -0.000000000000000000 ) ) ;
#5797 = DIRECTION ( 'NONE',  ( -1.000000000000000000, 0.000000000000000000, 0.000000000000000000 ) ) ;
#5798 = DIRECTION ( 'NONE',  ( 1.000000000000000000, 0.000000000000000000, 0.000000000000000000 ) ) ;
#5799 = CIRCLE ( 'NONE', #663, 0.4507874015748032370 ) ;
#5800 = CARTESIAN_POINT ( 'NONE',  ( 0.000000000000000000, 0.000000000000000000, 0.3732633159281743551 ) ) ;
#5801 = EDGE_CURVE ( 'NONE', #7420, #6581, #2030, .T. ) ;
#5802 = ADVANCED_FACE ( 'NONE', ( #233 ), #3712, .T. ) ;
#5803 = EDGE_CURVE ( 'NONE', #3252, #477, #6874, .T. ) ;
#5804 =( LENGTH_UNIT ( ) NAMED_UNIT ( * ) SI_UNIT ( $, .METRE. ) );
#5805 = CARTESIAN_POINT ( 'NONE',  ( 0.3425764178929370796, -0.2900721174007588332, -0.1006592143205869427 ) ) ;
#5806 = CARTESIAN_POINT ( 'NONE',  ( 0.000000000000000000, 0.000000000000000000, 0.000000000000000000 ) ) ;
#5807 = DIRECTION ( 'NONE',  ( 0.000000000000000000, 0.000000000000000000, -1.000000000000000000 ) ) ;
#5808 = EDGE_CURVE ( 'NONE', #6172, #4133, #6618, .T. ) ;
#5809 = EDGE_CURVE ( 'NONE', #5935, #408, #1487, .T. ) ;
#5810 = CARTESIAN_POINT ( 'NONE',  ( 0.3336175750056032396, -0.05682581389661664484, 0.2952755905511811330 ) ) ;
#5811 = DIRECTION ( 'NONE',  ( -1.000000000000000000, 0.000000000000000000, 0.000000000000000000 ) ) ;
#5812 = CARTESIAN_POINT ( 'NONE',  ( 0.002513486811083437498, 0.2845799557467908469, -0.09764423893321776127 ) ) ;
#5813 = DIRECTION ( 'NONE',  ( 1.000000000000000000, 0.000000000000000000, 0.000000000000000000 ) ) ;
#5814 = ORIENTED_EDGE ( 'NONE', *, *, #2929, .T. ) ;
#5815 = DIRECTION ( 'NONE',  ( 2.312579046053608732E-29, -2.207829878515936732E-15, -1.000000000000000000 ) ) ;
#5816 = SURFACE_STYLE_USAGE ( .BOTH. , #1009 ) ;
#5817 = ORIENTED_EDGE ( 'NONE', *, *, #3403, .T. ) ;
#5818 = VERTEX_POINT ( 'NONE', #1326 ) ;
#5819 = DIRECTION ( 'NONE',  ( 1.000000000000000000, 0.000000000000000000, 0.000000000000000000 ) ) ;
#5820 = AXIS2_PLACEMENT_3D ( 'NONE', #5578, #5076, #7393 ) ;
#5821 = DIRECTION ( 'NONE',  ( -1.000000000000000000, 1.224646799147353207E-16, 0.000000000000000000 ) ) ;
#5822 = ORIENTED_EDGE ( 'NONE', *, *, #5891, .F. ) ;
#5823 = CARTESIAN_POINT ( 'NONE',  ( 0.9541934910893004052, 0.4339190921229551523, -1.456692913385828847 ) ) ;
#5824 = B_SPLINE_CURVE_WITH_KNOTS ( 'NONE', 3,
 ( #7220, #5637, #3131, #7367, #2597, #7328 ),
 .UNSPECIFIED., .F., .F.,
 ( 4, 2, 4 ),
 ( -3.269571951033989319E-06, 0.0001651384380483822119, 0.0003335464480477984012 ),
 .UNSPECIFIED. ) ;
#5825 = CARTESIAN_POINT ( 'NONE',  ( 0.3483227611829848303, 0.3409548833797004797, 0.000000000000000000 ) ) ;
#5826 = CARTESIAN_POINT ( 'NONE',  ( -0.9917530546321610130, 0.4509662133831486841, -1.563429817131423372 ) ) ;
#5827 = EDGE_LOOP ( 'NONE', ( #5455, #6019 ) ) ;
#5828 = ORIENTED_EDGE ( 'NONE', *, *, #2103, .T. ) ;
#5829 = CARTESIAN_POINT ( 'NONE',  ( 0.3483227611829846637, 0.1704774416898499345, 0.2952755905511810774 ) ) ;
#5830 = CARTESIAN_POINT ( 'NONE',  ( -0.2073490933073312281, 0.2894328052184277356, -0.4082677165354333115 ) ) ;
#5831 = DIRECTION ( 'NONE',  ( -1.000000000000000000, 0.000000000000000000, 0.000000000000000000 ) ) ;
#5832 = CARTESIAN_POINT ( 'NONE',  ( 0.3483227611829846082, 0.1704774416898497680, -0.2952755905511810774 ) ) ;
#5833 = ORIENTED_EDGE ( 'NONE', *, *, #3553, .F. ) ;
#5834 = AXIS2_PLACEMENT_3D ( 'NONE', #1168, #2447, #4212 ) ;
#5835 = ADVANCED_FACE ( 'NONE', ( #6657 ), #1373, .T. ) ;
#5836 = CARTESIAN_POINT ( 'NONE',  ( 0.3483227611829848303, -0.1704774416898505729, -0.2952755905511810774 ) ) ;
#5837 = DIRECTION ( 'NONE',  ( 0.000000000000000000, 0.000000000000000000, -1.000000000000000000 ) ) ;
#5838 = AXIS2_PLACEMENT_3D ( 'NONE', #3790, #6662, #3755 ) ;
#5839 = DIRECTION ( 'NONE',  ( 0.000000000000000000, 1.000000000000000000, 0.000000000000000000 ) ) ;
#5840 = CARTESIAN_POINT ( 'NONE',  ( -0.9604263920613191896, 0.4330708661417286276, -1.456063616177414310 ) ) ;
#5841 = CARTESIAN_POINT ( 'NONE',  ( -0.4330708661417322913, 0.9697097892794930285, -1.453662943332487023 ) ) ;
#5842 = CARTESIAN_POINT ( 'NONE',  ( 0.000000000000000000, 0.000000000000000000, 0.000000000000000000 ) ) ;
#5843 = TOROIDAL_SURFACE ( 'NONE', #356, 1.223643328182682621, 0.05905511811023622659 ) ;
#5844 = EDGE_CURVE ( 'NONE', #3756, #3765, #168, .T. ) ;
#5845 = ADVANCED_FACE ( 'NONE', ( #2668 ), #2347, .T. ) ;
#5846 = DIRECTION ( 'NONE',  ( 0.000000000000000000, 0.000000000000000000, -1.000000000000000000 ) ) ;
#5847 = EDGE_LOOP ( 'NONE', ( #6427, #3920, #4251, #821 ) ) ;
#5848 = DIMENSIONAL_EXPONENTS ( 1.000000000000000000, 0.000000000000000000, 0.000000000000000000, 0.000000000000000000, 0.000000000000000000, 0.000000000000000000, 0.000000000000000000 ) ;
#5849 = CARTESIAN_POINT ( 'NONE',  ( 0.3410249605999410294, -1.062517223525361548E-12, -0.3014927230551905368 ) ) ;
#5850 = EDGE_CURVE ( 'NONE', #4833, #6826, #2952, .T. ) ;
#5851 = CARTESIAN_POINT ( 'NONE',  ( 0.000000000000000000, 0.2559055118110236116, 0.000000000000000000 ) ) ;
#5852 = CONICAL_SURFACE ( 'NONE', #5623, 0.4629062255509093782, 1.221730476396037490 ) ;
#5853 = VERTEX_POINT ( 'NONE', #764 ) ;
#5854 = EDGE_LOOP ( 'NONE', ( #3990, #5138 ) ) ;
#5855 = CARTESIAN_POINT ( 'NONE',  ( -0.3543307086614173040, 0.2045729300278199547, -0.03164754241312472960 ) ) ;
#5856 = AXIS2_PLACEMENT_3D ( 'NONE', #4028, #2300, #622 ) ;
#5857 = FACE_OUTER_BOUND ( 'NONE', #5544, .T. ) ;
#5858 = ORIENTED_EDGE ( 'NONE', *, *, #2891, .T. ) ;
#5859 = CARTESIAN_POINT ( 'NONE',  ( 0.3581828924050324825, -0.1743168766271116221, -0.3019256869348722061 ) ) ;
#5860 = FACE_OUTER_BOUND ( 'NONE', #2148, .T. ) ;
#5861 = ORIENTED_EDGE ( 'NONE', *, *, #5018, .F. ) ;
#5862 = VECTOR ( 'NONE', #3267, 39.37007874015748143 ) ;
#5863 = CARTESIAN_POINT ( 'NONE',  ( 0.000000000000000000, 1.496062992125984259, 0.000000000000000000 ) ) ;
#5864 = CARTESIAN_POINT ( 'NONE',  ( 0.3510870379221574522, 0.1475852640829200257, 0.2952755905511810774 ) ) ;
#5865 = APPLICATION_PROTOCOL_DEFINITION ( 'draft international standard', 'automotive_design', 1998, #3255 ) ;
#5866 = DIRECTION ( 'NONE',  ( 1.000000000000000000, 0.000000000000000000, 0.000000000000000000 ) ) ;
#5867 = CARTESIAN_POINT ( 'NONE',  ( 0.3496779098333545610, -0.1779789496721726760, 0.2952755905511811330 ) ) ;
#5868 = ADVANCED_BREP_SHAPE_REPRESENTATION ( '', ( #6540, #5166 ), #6134 ) ;
#5869 = DIRECTION ( 'NONE',  ( 1.000000000000000000, 0.000000000000000000, 0.000000000000000000 ) ) ;
#5870 = ORIENTED_EDGE ( 'NONE', *, *, #2383, .T. ) ;
#5871 = AXIS2_PLACEMENT_3D ( 'NONE', #4780, #4165, #6504 ) ;
#5872 = PRODUCT ( 'MAT-019', 'MAT-019', '', ( #1112 ) ) ;
#5873 = DIRECTION ( 'NONE',  ( -1.000000000000000000, 0.000000000000000000, 0.000000000000000000 ) ) ;
#5874 = CARTESIAN_POINT ( 'NONE',  ( -1.054581703806072746, 0.4332776154273863534, -1.572814851683855819 ) ) ;
#5875 = CARTESIAN_POINT ( 'NONE',  ( 0.000000000000000000, 0.000000000000000000, -2.204724409448820754 ) ) ;
#5876 = CIRCLE ( 'NONE', #6974, 0.4724409448818896462 ) ;
#5877 = CARTESIAN_POINT ( 'NONE',  ( 0.3496875133419357629, -0.1780312604149854316, -0.2952755905511810774 ) ) ;
#5878 = EDGE_CURVE ( 'NONE', #2266, #1419, #498, .T. ) ;
#5879 = CARTESIAN_POINT ( 'NONE',  ( -0.2362204724409449341, 2.892866454678787531E-17, -3.582716535433073002 ) ) ;
#5880 = CARTESIAN_POINT ( 'NONE',  ( -0.4999746636856473581, 0.9773775067402683536, -1.373988502838981107 ) ) ;
#5881 = LINE ( 'NONE', #5342, #5160 ) ;
#5882 = ITEM_DEFINED_TRANSFORMATION ( 'NONE', 'NONE', #2389,  #5166 ) ;
#5883 = CARTESIAN_POINT ( 'NONE',  ( 1.075170037517928723, 0.4403525121893840932, -1.561970602951606946 ) ) ;
#5884 = CIRCLE ( 'NONE', #2585, 0.2362204724409449619 ) ;
#5885 = CARTESIAN_POINT ( 'NONE',  ( 0.000000000000000000, 0.000000000000000000, 0.000000000000000000 ) ) ;
#5886 = CARTESIAN_POINT ( 'NONE',  ( 0.3432736861146661322, -0.1846838951640041859, 0.2706692913385828625 ) ) ;
#5887 = ORIENTED_EDGE ( 'NONE', *, *, #7378, .F. ) ;
#5888 = DIRECTION ( 'NONE',  ( 0.000000000000000000, -0.8660254037844379305, 0.5000000000000013323 ) ) ;
#5889 = DIRECTION ( 'NONE',  ( 0.000000000000000000, 0.000000000000000000, -1.000000000000000000 ) ) ;
#5890 = AXIS2_PLACEMENT_3D ( 'NONE', #5705, #5125, #5837 ) ;
#5891 = EDGE_CURVE ( 'NONE', #2124, #7498, #1234, .T. ) ;
#5892 = ADVANCED_FACE ( 'NONE', ( #5741 ), #7231, .T. ) ;
#5893 = ORIENTED_EDGE ( 'NONE', *, *, #5673, .T. ) ;
#5894 = CIRCLE ( 'NONE', #166, 0.3543307086614173596 ) ;
#5895 = EDGE_LOOP ( 'NONE', ( #6433, #6764, #4953, #5696, #1799 ) ) ;
#5896 = CARTESIAN_POINT ( 'NONE',  ( 0.7601524118086268045, -0.07627561187719542057, 0.9813965260305658189 ) ) ;
#5897 = EDGE_CURVE ( 'NONE', #7420, #450, #506, .T. ) ;
#5898 = AXIS2_PLACEMENT_3D ( 'NONE', #6053, #3783, #6085 ) ;
#5899 =( REPRESENTATION_RELATIONSHIP ('NONE','NONE', #303, #2147 ) REPRESENTATION_RELATIONSHIP_WITH_TRANSFORMATION ( #6197 )SHAPE_REPRESENTATION_RELATIONSHIP( ) );
#5900 = CARTESIAN_POINT ( 'NONE',  ( -0.3543307086614172485, 4.339299682018179447E-17, 0.3732633159281743551 ) ) ;
#5901 = ORIENTED_EDGE ( 'NONE', *, *, #3555, .F. ) ;
#5902 = LINE ( 'NONE', #6424, #5664 ) ;
#5903 = CARTESIAN_POINT ( 'NONE',  ( 0.3528971332113847725, 0.3341112492250003507, -0.02492269209175868722 ) ) ;
#5904 = EDGE_CURVE ( 'NONE', #1068, #1108, #3977, .T. ) ;
#5905 = VERTEX_POINT ( 'NONE', #5633 ) ;
#5906 = CIRCLE ( 'NONE', #6517, 1.074277634097406953 ) ;
#5907 = CARTESIAN_POINT ( 'NONE',  ( 0.3465694189147311421, -0.3147628225698668736, -0.04536598007755129891 ) ) ;
#5908 = PRODUCT_CONTEXT ( 'NONE', #2474, 'mechanical' ) ;
#5909 = FACE_OUTER_BOUND ( 'NONE', #7382, .T. ) ;
#5910 = CARTESIAN_POINT ( 'NONE',  ( 0.000000000000000000, 0.000000000000000000, 0.000000000000000000 ) ) ;
#5911 = EDGE_LOOP ( 'NONE', ( #1511, #7334, #741, #5870 ) ) ;
#5912 = CARTESIAN_POINT ( 'NONE',  ( -1.070877820178675721, -0.4996352642496130203, -1.498503547059352181 ) ) ;
#5913 = EDGE_LOOP ( 'NONE', ( #5486, #5473, #969, #3190 ) ) ;
#5914 = AXIS2_PLACEMENT_3D ( 'NONE', #6568, #1807, #1191 ) ;
#5915 = DIRECTION ( 'NONE',  ( 1.000000000000000000, 0.000000000000000000, 0.000000000000000000 ) ) ;
#5916 = ORIENTED_EDGE ( 'NONE', *, *, #1961, .T. ) ;
#5917 = AXIS2_PLACEMENT_3D ( 'NONE', #1404, #845, #2032 ) ;
#5918 = CARTESIAN_POINT ( 'NONE',  ( 0.3543307086614173596, 0.03458999977076016724, 3.421479542846110323E-17 ) ) ;
#5919 = CARTESIAN_POINT ( 'NONE',  ( 1.037563309807720380, 0.4338950423154246394, -1.574803149606299302 ) ) ;
#5920 = CARTESIAN_POINT ( 'NONE',  ( 0.000000000000000000, 0.000000000000000000, -1.574803149606299302 ) ) ;
#5921 = CARTESIAN_POINT ( 'NONE',  ( 7.874015748031496287, 0.2559055118110236116, 0.000000000000000000 ) ) ;
#5922 = AXIS2_PLACEMENT_3D ( 'NONE', #1727, #4065, #2303 ) ;
#5923 = DIRECTION ( 'NONE',  ( -1.000000000000000000, -0.000000000000000000, 0.000000000000000000 ) ) ;
#5924 = CARTESIAN_POINT ( 'NONE',  ( 0.4627504720074770983, -0.8884022185686297757, -1.439912370850674028 ) ) ;
#5925 = CARTESIAN_POINT ( 'NONE',  ( -1.037563309807723488, -0.4338950423154175340, -1.574803149606299302 ) ) ;
#5926 = DIRECTION ( 'NONE',  ( -0.000000000000000000, -0.000000000000000000, 1.000000000000000000 ) ) ;
#5927 = CARTESIAN_POINT ( 'NONE',  ( -1.704737175733852238E-16, 0.2629500981735131693, 0.1351082512106132616 ) ) ;
#5928 = PRODUCT_DEFINITION ( 'UNKNOWN', '', #5209, #1274 ) ;
#5929 = CARTESIAN_POINT ( 'NONE',  ( -2.834645669291338432, 0.000000000000000000, 2.952755905511811108 ) ) ;
#5930 = CARTESIAN_POINT ( 'NONE',  ( 0.3543307086614173040, -0.06891495372886456694, -0.4052962681128434164 ) ) ;
#5931 = DIRECTION ( 'NONE',  ( 2.204015539012438360E-32, 4.625929269271482167E-15, -1.000000000000000000 ) ) ;
#5932 = VERTEX_POINT ( 'NONE', #381 ) ;
#5933 = CARTESIAN_POINT ( 'NONE',  ( -0.4341579012690682804, -1.060348472569315303, -1.570964862939434825 ) ) ;
#5934 = CARTESIAN_POINT ( 'NONE',  ( 0.3997746709170348356, 0.000000000000000000, 0.000000000000000000 ) ) ;
#5935 = VERTEX_POINT ( 'NONE', #7403 ) ;
#5936 = ORIENTED_EDGE ( 'NONE', *, *, #6678, .T. ) ;
#5937 = CARTESIAN_POINT ( 'NONE',  ( 0.1023119647485438155, -0.3500760196667496715, -0.005786797686151859930 ) ) ;
#5938 = EDGE_CURVE ( 'NONE', #7488, #2228, #5706, .T. ) ;
#5939 = CARTESIAN_POINT ( 'NONE',  ( 0.4330708661417324024, 0.000000000000000000, 0.4507874015748032370 ) ) ;
#5940 = B_SPLINE_CURVE_WITH_KNOTS ( 'NONE', 3,
 ( #981, #6685, #5004, #2172, #3274, #3741, #6189, #4390, #910, #7252 ),
 .UNSPECIFIED., .F., .F.,
 ( 4, 2, 2, 2, 4 ),
 ( 0.000000000000000000, 0.0005216184974661249940, 0.001043236994932249988, 0.001564855492398375091, 0.002086473989864499976 ),
 .UNSPECIFIED. ) ;
#5941 = VERTEX_POINT ( 'NONE', #1551 ) ;
#5942 = CARTESIAN_POINT ( 'NONE',  ( 0.4330708661417322913, 0.9666437042230126009, -1.454455828411335583 ) ) ;
#5943 = CARTESIAN_POINT ( 'NONE',  ( 0.000000000000000000, 0.000000000000000000, -0.4082677165354330340 ) ) ;
#5944 = B_SPLINE_CURVE_WITH_KNOTS ( 'NONE', 3,
 ( #1245, #5398, #1285, #4820, #2321, #3051, #163, #1913, #74, #4656 ),
 .UNSPECIFIED., .F., .F.,
 ( 4, 2, 2, 2, 4 ),
 ( 0.000000000000000000, 0.002239656411828512290, 0.004479312823657024580, 0.006718969235485537303, 0.008958625647314049159 ),
 .UNSPECIFIED. ) ;
#5945 = EDGE_LOOP ( 'NONE', ( #3609, #1933, #5174, #7149, #2649, #3918 ) ) ;
#5946 = VERTEX_POINT ( 'NONE', #2216 ) ;
#5947 = CARTESIAN_POINT ( 'NONE',  ( 0.3581828924050323715, 0.1743168766271107895, -0.3019256869348722061 ) ) ;
#5948 = CARTESIAN_POINT ( 'NONE',  ( 0.3426404862726871725, 0.2904653615686527135, -0.09998168480679492376 ) ) ;
#5949 = EDGE_CURVE ( 'NONE', #6192, #3692, #6490, .T. ) ;
#5950 = EDGE_CURVE ( 'NONE', #408, #1972, #650, .T. ) ;
#5951 = FACE_OUTER_BOUND ( 'NONE', #4987, .T. ) ;
#5952 = CARTESIAN_POINT ( 'NONE',  ( -2.834645669291338432, 0.4724409448818890911, 8.169257281319195485 ) ) ;
#5953 = ORIENTED_EDGE ( 'NONE', *, *, #2330, .F. ) ;
#5954 = DIRECTION ( 'NONE',  ( -0.000000000000000000, -0.000000000000000000, 1.000000000000000000 ) ) ;
#5955 = ORIENTED_EDGE ( 'NONE', *, *, #3991, .T. ) ;
#5956 =( LENGTH_UNIT ( ) NAMED_UNIT ( * ) SI_UNIT ( $, .METRE. ) );
#5957 = ADVANCED_BREP_SHAPE_REPRESENTATION ( '', ( #3928, #5166 ), #4425 ) ;
#5958 = CARTESIAN_POINT ( 'NONE',  ( 0.3403864257300625029, -0.2851194846584945153, -0.09670974744601064377 ) ) ;
#5959 = CARTESIAN_POINT ( 'NONE',  ( 1.048552902599924730, -0.4330708661417213001, -1.573978973432616835 ) ) ;
#5960 = CARTESIAN_POINT ( 'NONE',  ( 0.9842519685039370358, 1.220472440944881942, 2.952755905511811108 ) ) ;
#5961 = PRODUCT_DEFINITION_CONTEXT ( 'detailed design', #3004, 'design' ) ;
#5962 = CARTESIAN_POINT ( 'NONE',  ( -0.4349482548737262921, -1.030265823844199069, -1.574803149606299746 ) ) ;
#5963 = DIRECTION ( 'NONE',  ( 0.000000000000000000, 0.000000000000000000, 1.000000000000000000 ) ) ;
#5964 = CARTESIAN_POINT ( 'NONE',  ( 0.3336175750056032396, 0.2841290694830835850, 0.09842519685039366473 ) ) ;
#5965 = CARTESIAN_POINT ( 'NONE',  ( 2.755905511811024056, 0.000000000000000000, 0.2362204724409449896 ) ) ;
#5966 = B_SPLINE_CURVE_WITH_KNOTS ( 'NONE', 3,
 ( #4845, #5927, #2589, #1321, #4772, #684, #759, #4927 ),
 .UNSPECIFIED., .F., .F.,
 ( 4, 2, 2, 4 ),
 ( 0.004381617662950689981, 0.005472867551409524994, 0.006564117439868360007, 0.008746617216786028298 ),
 .UNSPECIFIED. ) ;
#5967 = CONICAL_SURFACE ( 'NONE', #5838, 0.1982677165354330695, 0.7853981633974415066 ) ;
#5968 = CARTESIAN_POINT ( 'NONE',  ( 0.3391892065151630442, -0.3125419764313924764, -0.04921259842519686706 ) ) ;
#5969 = CARTESIAN_POINT ( 'NONE',  ( 1.037563309807729262, -0.4338950423154036007, -1.574803149606299302 ) ) ;
#5970 = DIRECTION ( 'NONE',  ( 1.000000000000000000, 0.000000000000000000, 0.000000000000000000 ) ) ;
#5971 = VERTEX_POINT ( 'NONE', #5087 ) ;
#5972 = CARTESIAN_POINT ( 'NONE',  ( -0.4630669964643905900, -1.085749034322389894, -1.535808346805854541 ) ) ;
#5973 = DIRECTION ( 'NONE',  ( 0.000000000000000000, 1.000000000000000000, 0.000000000000000000 ) ) ;
#5974 = VERTEX_POINT ( 'NONE', #425 ) ;
#5975 = AXIS2_PLACEMENT_3D ( 'NONE', #2761, #2969, #1614 ) ;
#5976 = CARTESIAN_POINT ( 'NONE',  ( 0.000000000000000000, 1.496062992125984259, 0.000000000000000000 ) ) ;
#5977 = CARTESIAN_POINT ( 'NONE',  ( 0.000000000000000000, 0.000000000000000000, -0.4921259842519685179 ) ) ;
#5978 = ORIENTED_EDGE ( 'NONE', *, *, #7152, .F. ) ;
#5979 = CIRCLE ( 'NONE', #6945, 0.2362204724409448231 ) ;
#5980 = DIRECTION ( 'NONE',  ( -1.000000000000000000, 0.000000000000000000, 0.000000000000000000 ) ) ;
#5981 = ORIENTED_EDGE ( 'NONE', *, *, #6368, .F. ) ;
#5982 = PRODUCT_DEFINITION ( 'UNKNOWN', '', #2273, #3041 ) ;
#5983 = ORIENTED_EDGE ( 'NONE', *, *, #1483, .T. ) ;
#5984 = CARTESIAN_POINT ( 'NONE',  ( 1.220472440944881720, 0.000000000000000000, -1.377952755905512028 ) ) ;
#5985 = AXIS2_PLACEMENT_3D ( 'NONE', #7417, #5687, #3374 ) ;
#5986 = CARTESIAN_POINT ( 'NONE',  ( 0.3391221370943153790, -0.1204748818123362597, 0.2952755905511811330 ) ) ;
#5987 = SHAPE_DEFINITION_REPRESENTATION ( #72, #1552 ) ;
#5988 = FACE_OUTER_BOUND ( 'NONE', #2346, .T. ) ;
#5989 = CARTESIAN_POINT ( 'NONE',  ( -0.4353079511162236681, -0.9479499796399322165, -1.456692913385828625 ) ) ;
#5990 = DIRECTION ( 'NONE',  ( 0.000000000000000000, 0.000000000000000000, 1.000000000000000000 ) ) ;
#5991 = VECTOR ( 'NONE', #4308, 39.37007874015748143 ) ;
#5992 = CARTESIAN_POINT ( 'NONE',  ( 0.3483227611829846637, -0.1704774416898499345, 0.2952755905511811330 ) ) ;
#5993 = ADVANCED_FACE ( 'NONE', ( #7364 ), #3360, .F. ) ;
#5994 = ORIENTED_EDGE ( 'NONE', *, *, #7461, .F. ) ;
#5995 = EDGE_CURVE ( 'NONE', #5757, #4791, #4561, .T. ) ;
#5996=STYLED_ITEM('',(#7559),#3928);
#5997 = CARTESIAN_POINT ( 'NONE',  ( 0.3479980290963871625, -0.2016732288369692816, -0.2541005850305417257 ) ) ;
#5998 = DIRECTION ( 'NONE',  ( -0.000000000000000000, -0.000000000000000000, -1.000000000000000000 ) ) ;
#5999 = AXIS2_PLACEMENT_3D ( 'NONE', #3551, #6544, #727 ) ;
#6000 = ADVANCED_FACE ( 'NONE', ( #4585 ), #5164, .T. ) ;
#6001 =( REPRESENTATION_RELATIONSHIP ('NONE','NONE', #303, #2912 ) REPRESENTATION_RELATIONSHIP_WITH_TRANSFORMATION ( #4553 )SHAPE_REPRESENTATION_RELATIONSHIP( ) );
#6002 = CARTESIAN_POINT ( 'NONE',  ( -0.9479499796399322165, 0.4353079511162203374, -1.456692913385826849 ) ) ;
#6003 = PLANE ( 'NONE',  #1346 ) ;
#6004 = ITEM_DEFINED_TRANSFORMATION ( 'NONE', 'NONE', #5094,  #5166 ) ;
#6005 = TOROIDAL_SURFACE ( 'NONE', #380, 1.124634398195722973, 0.05905511811023622659 ) ;
#6006 = CARTESIAN_POINT ( 'NONE',  ( 0.002549129251883240199, 0.05807386165065146072, -0.2952755905511810219 ) ) ;
#6007 = CARTESIAN_POINT ( 'NONE',  ( -0.3543307086614173040, -0.2045729300278205931, -0.03164754241312491001 ) ) ;
#6008 = LINE ( 'NONE', #7175, #1563 ) ;
#6009 = EDGE_LOOP ( 'NONE', ( #2194, #1401, #2505, #7348 ) ) ;
#6010 = PRODUCT ( 'hex flange bolt small_iso_ISO 4162 - M12 x 65 x 65-N', 'hex flange bolt small_iso_ISO 4162 - M12 x 65 x 65-N', '', ( #5596 ) ) ;
#6011 = DIRECTION ( 'NONE',  ( -1.000000000000000000, -1.049299683535327448E-14, 0.000000000000000000 ) ) ;
#6012 = CARTESIAN_POINT ( 'NONE',  ( 2.834645669291338876, 0.4724409448818890911, 2.480314960629921295 ) ) ;
#6013 = ORIENTED_EDGE ( 'NONE', *, *, #1931, .T. ) ;
#6014 = AXIS2_PLACEMENT_3D ( 'NONE', #4197, #4116, #4082 ) ;
#6015 = VECTOR ( 'NONE', #5699, 39.37007874015748143 ) ;
#6016 = CARTESIAN_POINT ( 'NONE',  ( 0.4330708661417324024, 0.000000000000000000, 0.000000000000000000 ) ) ;
#6017 = FACE_OUTER_BOUND ( 'NONE', #3680, .T. ) ;
#6018 = AXIS2_PLACEMENT_3D ( 'NONE', #6479, #2422, #1733 ) ;
#6019 = ORIENTED_EDGE ( 'NONE', *, *, #2987, .T. ) ;
#6020 = DIRECTION ( 'NONE',  ( 0.000000000000000000, 0.000000000000000000, -1.000000000000000000 ) ) ;
#6021 = ORIENTED_EDGE ( 'NONE', *, *, #2711, .T. ) ;
#6022 = ORIENTED_EDGE ( 'NONE', *, *, #5325, .F. ) ;
#6023 = AXIS2_PLACEMENT_3D ( 'NONE', #6860, #2802, #523 ) ;
#6024 = CARTESIAN_POINT ( 'NONE',  ( 0.3565325103478086954, -0.1673557731150450700, -0.3006824791271353603 ) ) ;
#6025 = EDGE_LOOP ( 'NONE', ( #5901, #2955, #6022, #6783, #960, #4187 ) ) ;
#6026 = CARTESIAN_POINT ( 'NONE',  ( 0.3510872220067180471, 0.3295092824291462330, 0.01982436236955231745 ) ) ;
#6027 = VERTEX_POINT ( 'NONE', #7440 ) ;
#6028 = CARTESIAN_POINT ( 'NONE',  ( -0.4700904924197908397, -0.8785537298370134085, -1.433776001880364470 ) ) ;
#6029 = PRODUCT_DEFINITION ( 'UNKNOWN', '', #3248, #1816 ) ;
#6030 = ORIENTED_EDGE ( 'NONE', *, *, #2891, .F. ) ;
#6031 = AXIS2_PLACEMENT_3D ( 'NONE', #4978, #7297, #3834 ) ;
#6032 = CARTESIAN_POINT ( 'NONE',  ( 0.3426404862726872280, -0.2904653615686530466, 0.09998168480679490988 ) ) ;
#6033 = VERTEX_POINT ( 'NONE', #5127 ) ;
#6034 = CARTESIAN_POINT ( 'NONE',  ( 0.003035684155427393477, -0.2845908893795038308, -0.09762530132584867903 ) ) ;
#6035 = CARTESIAN_POINT ( 'NONE',  ( -2.834645669291338432, 0.4724409448818898127, 2.952755905511811108 ) ) ;
#6036=STYLED_ITEM('',(#7594),#1517);
#6037 = ADVANCED_FACE ( 'NONE', ( #3435 ), #5775, .F. ) ;
#6038 = ADVANCED_FACE ( 'NONE', ( #4434 ), #4804, .T. ) ;
#6039 = CARTESIAN_POINT ( 'NONE',  ( -0.8833138556570234723, -0.4663806185493133416, -1.436938405272265573 ) ) ;
#6040 = CARTESIAN_POINT ( 'NONE',  ( 0.000000000000000000, 1.496062992125984259, 0.7480314960629921295 ) ) ;
#6041 = ADVANCED_FACE ( 'NONE', ( #2707 ), #5050, .F. ) ;
#6042 = UNCERTAINTY_MEASURE_WITH_UNIT (LENGTH_MEASURE( 1.000000000000000082E-05 ), #4107, 'distance_accuracy_value', 'NONE');
#6043 = DIRECTION ( 'NONE',  ( 0.000000000000000000, 0.000000000000000000, -1.000000000000000000 ) ) ;
#6044 = DIRECTION ( 'NONE',  ( 0.000000000000000000, 0.000000000000000000, 1.000000000000000000 ) ) ;
#6045 = CARTESIAN_POINT ( 'NONE',  ( 0.000000000000000000, -0.2557161625347750822, -0.1476377952755907330 ) ) ;
#6046 = ADVANCED_FACE ( 'NONE', ( #2312 ), #6133, .F. ) ;
#6047 = DIRECTION ( 'NONE',  ( 0.000000000000000000, 1.000000000000000000, 0.000000000000000000 ) ) ;
#6048 = CARTESIAN_POINT ( 'NONE',  ( 0.3581828924050323715, -0.1743168766271109560, 0.3019256869348722616 ) ) ;
#6049 = LINE ( 'NONE', #3091, #5616 ) ;
#6050 = EDGE_CURVE ( 'NONE', #4943, #2367, #294, .T. ) ;
#6051 = ORIENTED_EDGE ( 'NONE', *, *, #5281, .F. ) ;
#6052 = VECTOR ( 'NONE', #5384, 39.37007874015748143 ) ;
#6053 = CARTESIAN_POINT ( 'NONE',  ( -0.4700904924197872314, 0.000000000000000000, -2.204724409448822975 ) ) ;
#6054 = CARTESIAN_POINT ( 'NONE',  ( -0.4375700573520698300, 1.070856907295305804, -1.565644078513316106 ) ) ;
#6055 = APPLICATION_CONTEXT ( 'automotive_design' ) ;
#6056 = ORIENTED_EDGE ( 'NONE', *, *, #706, .T. ) ;
#6057 = CARTESIAN_POINT ( 'NONE',  ( -2.349015779708382802E-16, 0.2702383257424525453, -0.1224846707640857985 ) ) ;
#6058 = CARTESIAN_POINT ( 'NONE',  ( 0.3531513458567848707, -0.1471090214728858203, -0.3018164116569697075 ) ) ;
#6059 = DIRECTION ( 'NONE',  ( 0.000000000000000000, 1.000000000000000000, 0.000000000000000000 ) ) ;
#6060 = CARTESIAN_POINT ( 'NONE',  ( 1.170506159394721758E-17, 0.02884736746562922144, 0.2952755905511810774 ) ) ;
#6061 = ORIENTED_EDGE ( 'NONE', *, *, #5684, .F. ) ;
#6062 = CARTESIAN_POINT ( 'NONE',  ( 0.000000000000000000, 0.2559055118110236116, -0.4921259842519685179 ) ) ;
#6063 = ORIENTED_EDGE ( 'NONE', *, *, #2060, .T. ) ;
#6064 = CARTESIAN_POINT ( 'NONE',  ( 0.3487102105009288744, -0.3201373431253433655, -0.04891434758976972302 ) ) ;
#6065 = DIRECTION ( 'NONE',  ( 1.000000000000000000, 0.000000000000000000, 0.000000000000000000 ) ) ;
#6066 = CARTESIAN_POINT ( 'NONE',  ( 0.9883301303667366700, -0.4377665650305532230, -1.443420399700354295 ) ) ;
#6067 = ORIENTED_EDGE ( 'NONE', *, *, #5950, .F. ) ;
#6068 = CARTESIAN_POINT ( 'NONE',  ( 0.7556465724085326130, 0.06151677279835152806, 0.9824476696380366469 ) ) ;
#6069 = ORIENTED_EDGE ( 'NONE', *, *, #3703, .F. ) ;
#6070 = DIRECTION ( 'NONE',  ( -1.776356839400250465E-15, 1.000000000000000000, -2.256009703088257329E-15 ) ) ;
#6071 = EDGE_LOOP ( 'NONE', ( #6748, #2288, #5258, #4365, #5978, #3728 ) ) ;
#6072 = PRODUCT_DEFINITION_SHAPE ( 'NONE', 'NONE',  #7552 ) ;
#6073 = CARTESIAN_POINT ( 'NONE',  ( 1.037563309807729262, -0.4338950423154036007, -1.574803149606299302 ) ) ;
#6074 = CARTESIAN_POINT ( 'NONE',  ( 0.7965271477292853453, -0.1442139612367993318, -0.9737154292565876057 ) ) ;
#6075 = PRODUCT_DEFINITION_FORMATION_WITH_SPECIFIED_SOURCE ( 'ANY', '', #5872, .NOT_KNOWN. ) ;
#6076 = DIRECTION ( 'NONE',  ( 0.000000000000000000, 0.000000000000000000, -1.000000000000000000 ) ) ;
#6077 = ADVANCED_FACE ( 'NONE', ( #3003 ), #7239, .T. ) ;
#6078 = CARTESIAN_POINT ( 'NONE',  ( 7.874015748031496287, 0.2559055118110236116, 0.000000000000000000 ) ) ;
#6079 = FACE_OUTER_BOUND ( 'NONE', #6823, .T. ) ;
#6080 = CARTESIAN_POINT ( 'NONE',  ( 0.01841426102874111140, 0.1429077274040426171, -0.2952755905511810219 ) ) ;
#6081 = CARTESIAN_POINT ( 'NONE',  ( 0.02637295201093697167, 0.1704774416898497680, -0.2952755905511810774 ) ) ;
#6082 = FACE_OUTER_BOUND ( 'NONE', #3335, .T. ) ;
#6083 = PLANE ( 'NONE',  #594 ) ;
#6084 = ORIENTED_EDGE ( 'NONE', *, *, #983, .T. ) ;
#6085 = DIRECTION ( 'NONE',  ( 4.615976749461840186E-15, 0.000000000000000000, -1.000000000000000000 ) ) ;
#6086 = DIRECTION ( 'NONE',  ( -1.000000000000000000, 0.000000000000000000, 0.000000000000000000 ) ) ;
#6087 = VERTEX_POINT ( 'NONE', #7056 ) ;
#6088 = DIRECTION ( 'NONE',  ( -0.000000000000000000, -1.000000000000000000, 0.000000000000000000 ) ) ;
#6089 = EDGE_CURVE ( 'NONE', #4786, #2154, #7099, .T. ) ;
#6090 = EDGE_CURVE ( 'NONE', #1132, #1529, #2918, .T. ) ;
#6091 = FACE_OUTER_BOUND ( 'NONE', #6959, .T. ) ;
#6092 = ADVANCED_FACE ( 'NONE', ( #3470 ), #579, .F. ) ;
#6093 = CARTESIAN_POINT ( 'NONE',  ( 0.5072158114890842340, 1.064252964791788658, -1.491281854710626575 ) ) ;
#6094 = ORIENTED_EDGE ( 'NONE', *, *, #7243, .F. ) ;
#6095 = CARTESIAN_POINT ( 'NONE',  ( 0.3561392902752972267, -0.1723302545757742776, 0.2984847566065203517 ) ) ;
#6096 = CIRCLE ( 'NONE', #6829, 0.2362204724409448231 ) ;
#6097 = ORIENTED_EDGE ( 'NONE', *, *, #5242, .F. ) ;
#6098 = ORIENTED_EDGE ( 'NONE', *, *, #1731, .F. ) ;
#6099 = CARTESIAN_POINT ( 'NONE',  ( 1.968503937007874072, 0.000000000000000000, 0.000000000000000000 ) ) ;
#6100 = AXIS2_PLACEMENT_3D ( 'NONE', #2950, #2379, #2993 ) ;
#6101 = CARTESIAN_POINT ( 'NONE',  ( 0.004822332172886236931, -0.2197023059474404461, 0.2100156246613535393 ) ) ;
#6102 = FACE_OUTER_BOUND ( 'NONE', #2235, .T. ) ;
#6103 = ORIENTED_EDGE ( 'NONE', *, *, #4625, .T. ) ;
#6104 = CARTESIAN_POINT ( 'NONE',  ( 0.3505602286436571569, 0.3409548833797004797, 4.673058124370679309E-18 ) ) ;
#6105 = CARTESIAN_POINT ( 'NONE',  ( 0.3410076799406686066, -0.2467857494855110190, 0.1755389823809323790 ) ) ;
#6106 = AXIS2_PLACEMENT_3D ( 'NONE', #1821, #3087, #3009 ) ;
#6107 = CARTESIAN_POINT ( 'NONE',  ( 0.2699662542182227343, 0.000000000000000000, 0.1188976377952756375 ) ) ;
#6108 = CARTESIAN_POINT ( 'NONE',  ( 1.121892893784558254, -0.1921327968434894951, -0.9653269806155788668 ) ) ;
#6109 = AXIS2_PLACEMENT_3D ( 'NONE', #259, #6793, #336 ) ;
#6110 = CARTESIAN_POINT ( 'NONE',  ( -0.8989365377700702098, -0.4559220466128956484, -1.445239289764782997 ) ) ;
#6111 = CIRCLE ( 'NONE', #4637, 0.2952755905511810774 ) ;
#6112 = FACE_OUTER_BOUND ( 'NONE', #809, .T. ) ;
#6113 = DIRECTION ( 'NONE',  ( 0.000000000000000000, 0.000000000000000000, -1.000000000000000000 ) ) ;
#6114 = CARTESIAN_POINT ( 'NONE',  ( 0.3410076799406683290, 0.2754140928391118348, 0.1259532371559686781 ) ) ;
#6115 = ORIENTED_EDGE ( 'NONE', *, *, #1343, .T. ) ;
#6116 = CARTESIAN_POINT ( 'NONE',  ( -0.9666437042230142662, 0.4330708661417289052, -1.454455828411335583 ) ) ;
#6117 = EDGE_CURVE ( 'NONE', #5247, #5932, #2278, .T. ) ;
#6118 = CARTESIAN_POINT ( 'NONE',  ( 0.3527008206095850751, 0.3418447298186451655, 4.692841048826145323E-17 ) ) ;
#6119 = CARTESIAN_POINT ( 'NONE',  ( 0.000000000000000000, 0.2557161625347749712, -0.1476377952755909551 ) ) ;
#6120 = DIRECTION ( 'NONE',  ( -1.000000000000000000, 0.000000000000000000, 0.000000000000000000 ) ) ;
#6121 = AXIS2_PLACEMENT_3D ( 'NONE', #690, #3013, #5351 ) ;
#6122 = DIRECTION ( 'NONE',  ( 0.000000000000000000, 0.000000000000000000, -1.000000000000000000 ) ) ;
#6123 = ORIENTED_EDGE ( 'NONE', *, *, #4615, .F. ) ;
#6124 = DIRECTION ( 'NONE',  ( -1.000000000000000000, 0.000000000000000000, 0.000000000000000000 ) ) ;
#6125 = EDGE_CURVE ( 'NONE', #2228, #5565, #5227, .T. ) ;
#6126 = EDGE_CURVE ( 'NONE', #2217, #321, #3001, .T. ) ;
#6127 = CIRCLE ( 'NONE', #2819, 0.4921259842519685179 ) ;
#6128 = ORIENTED_EDGE ( 'NONE', *, *, #5334, .F. ) ;
#6129 = PRODUCT_DEFINITION_SHAPE ( 'NONE', 'NONE',  #7539 ) ;
#6130 = VERTEX_POINT ( 'NONE', #5960 ) ;
#6131 = EDGE_CURVE ( 'NONE', #630, #443, #5906, .T. ) ;
#6132 = CARTESIAN_POINT ( 'NONE',  ( 0.01834252172841674411, -0.3270457701237520221, -0.02409129084753309710 ) ) ;
#6133 = CONICAL_SURFACE ( 'NONE', #5548, 0.2362204724409449619, 0.9599310885968795892 ) ;
#6134 =( GEOMETRIC_REPRESENTATION_CONTEXT ( 3 ) GLOBAL_UNCERTAINTY_ASSIGNED_CONTEXT ( ( #224 ) ) GLOBAL_UNIT_ASSIGNED_CONTEXT ( ( #1420, #2618, #4306 ) ) REPRESENTATION_CONTEXT ( 'NONE', 'WORKASPACE' ) );
#6135 = CARTESIAN_POINT ( 'NONE',  ( 0.02637295201093707228, -0.1704774416898499345, 0.2952755905511811330 ) ) ;
#6136 = CARTESIAN_POINT ( 'NONE',  ( 0.3322361761492683696, 0.2247851515112334331, 0.2012118778978378431 ) ) ;
#6137 = VERTEX_POINT ( 'NONE', #6947 ) ;
#6138 = CIRCLE ( 'NONE', #4545, 1.968503937007874072 ) ;
#6139 = CARTESIAN_POINT ( 'NONE',  ( 0.3432736861146661878, -0.1420645347415422088, -0.2952755905511810774 ) ) ;
#6140 = ORIENTED_EDGE ( 'NONE', *, *, #1589, .F. ) ;
#6141 = ADVANCED_FACE ( 'NONE', ( #6984 ), #1737, .F. ) ;
#6142 = CARTESIAN_POINT ( 'NONE',  ( 0.3321022367506963890, 0.2702568778840441777, 0.1224525375122600818 ) ) ;
#6143 = ORIENTED_EDGE ( 'NONE', *, *, #7005, .T. ) ;
#6144 = VECTOR ( 'NONE', #4763, 39.37007874015748143 ) ;
#6145 = ORIENTED_EDGE ( 'NONE', *, *, #2769, .F. ) ;
#6146 = B_SPLINE_CURVE_WITH_KNOTS ( 'NONE', 3,
 ( #5989, #1340, #4677, #16 ),
 .UNSPECIFIED., .F., .F.,
 ( 4, 4 ),
 ( 0.000000000000000000, 0.0004815725036528575279 ),
 .UNSPECIFIED. ) ;
#6147 = DIRECTION ( 'NONE',  ( 1.000000000000000000, 0.000000000000000000, 0.000000000000000000 ) ) ;
#6148 = DIRECTION ( 'NONE',  ( 1.000000000000000000, 0.000000000000000000, 0.000000000000000000 ) ) ;
#6149 = CARTESIAN_POINT ( 'NONE',  ( 1.089019577240956993, -0.2122777770860161672, -0.9611070884360988220 ) ) ;
#6150 = CIRCLE ( 'NONE', #2343, 1.223643328182681289 ) ;
#6151 =( REPRESENTATION_RELATIONSHIP ('NONE','NONE', #303, #1307 ) REPRESENTATION_RELATIONSHIP_WITH_TRANSFORMATION ( #388 )SHAPE_REPRESENTATION_RELATIONSHIP( ) );
#6152 = CARTESIAN_POINT ( 'NONE',  ( 0.02637295201093707228, -0.1704774416898499345, 0.2952755905511811330 ) ) ;
#6153 = AXIS2_PLACEMENT_3D ( 'NONE', #4079, #866, #4311 ) ;
#6154 = DIRECTION ( 'NONE',  ( 7.708596820178695308E-30, -2.207829878515936732E-15, 1.000000000000000000 ) ) ;
#6155 = CARTESIAN_POINT ( 'NONE',  ( 0.3483227611829848303, 0.3409548833797004797, 0.000000000000000000 ) ) ;
#6156 = CARTESIAN_POINT ( 'NONE',  ( -1.704737175733852238E-16, 0.2629500981735131693, 0.1351082512106132616 ) ) ;
#6157 = CARTESIAN_POINT ( 'NONE',  ( -0.4700904924197902846, 0.9659644734970543878, -1.546597720061111847 ) ) ;
#6158 = ORIENTED_EDGE ( 'NONE', *, *, #3456, .F. ) ;
#6159 = B_SPLINE_CURVE_WITH_KNOTS ( 'NONE', 3,
 ( #2437, #4770, #5433, #4156, #4236, #7106, #189, #2511, #7209, #6497, #5388, #5883, #4844, #1866, #7170, #4272, #6610, #67 ),
 .UNSPECIFIED., .F., .F.,
 ( 4, 2, 2, 2, 2, 2, 2, 2, 4 ),
 ( -8.042425861379543572E-06, 0.0009212656149224119229, 0.001385919635314298778, 0.001850573655706185634, 0.002315227676098072923, 0.002779881696489959562, 0.003244535716881846200, 0.003476862727077784532, 0.003709189737273723732 ),
 .UNSPECIFIED. ) ;
#6160 = DIRECTION ( 'NONE',  ( -1.000000000000000000, 0.000000000000000000, 0.000000000000000000 ) ) ;
#6161 = CARTESIAN_POINT ( 'NONE',  ( -0.1023119647485438294, 0.3500760196667492274, -0.005786797686151529466 ) ) ;
#6162 = CARTESIAN_POINT ( 'NONE',  ( 0.3585569304025113535, 0.1763492631043844516, -0.3019338371022697864 ) ) ;
#6163 = VECTOR ( 'NONE', #755, 39.37007874015748143 ) ;
#6164 = CARTESIAN_POINT ( 'NONE',  ( 0.4375700573520702741, 1.070856907295305804, -1.565644078513316773 ) ) ;
#6165 = ORIENTED_EDGE ( 'NONE', *, *, #5622, .T. ) ;
#6166 = CARTESIAN_POINT ( 'NONE',  ( 0.5141614760841458631, 1.056523642887403192, -1.484898342931014303 ) ) ;
#6167 = ORIENTED_EDGE ( 'NONE', *, *, #7191, .T. ) ;
#6168 = ORIENTED_EDGE ( 'NONE', *, *, #4997, .F. ) ;
#6169 = DIRECTION ( 'NONE',  ( 0.000000000000000000, -1.001543065824774208E-16, -1.000000000000000000 ) ) ;
#6170 = DIRECTION ( 'NONE',  ( -1.000000000000000000, 0.000000000000000000, 0.000000000000000000 ) ) ;
#6171 = EDGE_CURVE ( 'NONE', #6027, #4478, #4757, .T. ) ;
#6172 = VERTEX_POINT ( 'NONE', #3199 ) ;
#6173 = CARTESIAN_POINT ( 'NONE',  ( 0.9810556462971189440, -0.4349192958999650305, -1.448591228719267487 ) ) ;
#6174 = ORIENTED_EDGE ( 'NONE', *, *, #51, .T. ) ;
#6175 = CARTESIAN_POINT ( 'NONE',  ( 1.015122112586412939, 0.2347042945180431994, 0.9558637132201285302 ) ) ;
#6176 = DIRECTION ( 'NONE',  ( -0.000000000000000000, -0.000000000000000000, 1.000000000000000000 ) ) ;
#6177 = ORIENTED_EDGE ( 'NONE', *, *, #5542, .F. ) ;
#6178 = ORIENTED_EDGE ( 'NONE', *, *, #6353, .F. ) ;
#6179 = ADVANCED_FACE ( 'NONE', ( #5464 ), #7480, .T. ) ;
#6180 = EDGE_CURVE ( 'NONE', #4020, #7296, #117, .T. ) ;
#6181 = CARTESIAN_POINT ( 'NONE',  ( 27.32692456122369151, 45.20863634146751764, 51.90956403617311565 ) ) ;
#6182 = CARTESIAN_POINT ( 'NONE',  ( 2.834645669291338432, 0.000000000000000000, 0.000000000000000000 ) ) ;
#6183 = CARTESIAN_POINT ( 'NONE',  ( 1.060520566440911416, -0.2241008867759824719, -0.9584192624488059309 ) ) ;
#6184 = EDGE_CURVE ( 'NONE', #3879, #2077, #898, .T. ) ;
#6185 = FACE_BOUND ( 'NONE', #2370, .T. ) ;
#6186 = CARTESIAN_POINT ( 'NONE',  ( 0.7794093496269024479, 0.1186414295356391785, -0.9771602695683655471 ) ) ;
#6187 = CARTESIAN_POINT ( 'NONE',  ( 0.4368380215374126352, 1.023371766162644914, -1.573834103987475475 ) ) ;
#6188 = AXIS2_PLACEMENT_3D ( 'NONE', #6938, #529, #5831 ) ;
#6189 = CARTESIAN_POINT ( 'NONE',  ( 0.4559215864680338792, 0.8989373009621102195, -1.445239633971734383 ) ) ;
#6190 = CARTESIAN_POINT ( 'NONE',  ( 0.4685039370078740717, -0.1704774416898505729, -0.2952755905511810774 ) ) ;
#6191 = DIRECTION ( 'NONE',  ( 1.000000000000000000, 1.047444401652940007E-14, 0.000000000000000000 ) ) ;
#6192 = VERTEX_POINT ( 'NONE', #4881 ) ;
#6193 = DIRECTION ( 'NONE',  ( 1.000000000000000000, 0.000000000000000000, 0.000000000000000000 ) ) ;
#6194 = VECTOR ( 'NONE', #1413, 39.37007874015748143 ) ;
#6195 = ORIENTED_EDGE ( 'NONE', *, *, #1536, .F. ) ;
#6196 = LINE ( 'NONE', #5879, #6163 ) ;
#6197 = ITEM_DEFINED_TRANSFORMATION ( 'NONE', 'NONE', #3696,  #5166 ) ;
#6198 = CARTESIAN_POINT ( 'NONE',  ( 0.3336175750056034617, -0.2841290694830840846, -0.09842519685039370636 ) ) ;
#6199 = ORIENTED_EDGE ( 'NONE', *, *, #4822, .F. ) ;
#6200 = DIRECTION ( 'NONE',  ( -0.000000000000000000, -0.000000000000000000, 1.000000000000000000 ) ) ;
#6201 = FACE_OUTER_BOUND ( 'NONE', #6025, .T. ) ;
#6202 = ORIENTED_EDGE ( 'NONE', *, *, #6492, .T. ) ;
#6203 = VECTOR ( 'NONE', #3689, 39.37007874015748143 ) ;
#6204 = ORIENTED_EDGE ( 'NONE', *, *, #2855, .T. ) ;
#6205 = DIRECTION ( 'NONE',  ( -0.000000000000000000, -1.000000000000000000, -0.000000000000000000 ) ) ;
#6206 = LINE ( 'NONE', #968, #2170 ) ;
#6207 = ORIENTED_EDGE ( 'NONE', *, *, #1589, .T. ) ;
#6208 = CARTESIAN_POINT ( 'NONE',  ( 0.000000000000000000, 1.496062992125984259, 0.000000000000000000 ) ) ;
#6209 = VERTEX_POINT ( 'NONE', #1314 ) ;
#6210 = AXIS2_PLACEMENT_3D ( 'NONE', #3357, #2212, #3241 ) ;
#6211 = CARTESIAN_POINT ( 'NONE',  ( -0.3543307086614172485, 4.339299682018179447E-17, 0.1188976377952756375 ) ) ;
#6212 = B_SPLINE_CURVE_WITH_KNOTS ( 'NONE', 3,
 ( #5925, #5306, #2436, #2922 ),
 .UNSPECIFIED., .F., .F.,
 ( 4, 4 ),
 ( 6.648767611728001586E-17, 0.0002807012396508847571 ),
 .UNSPECIFIED. ) ;
#6213 = CARTESIAN_POINT ( 'NONE',  ( 0.3510872220067180471, 0.3295092824291462330, 0.01982436236955231745 ) ) ;
#6214 = ORIENTED_EDGE ( 'NONE', *, *, #1920, .T. ) ;
#6215 = CARTESIAN_POINT ( 'NONE',  ( 0.01841426102874111140, 0.1429077274040426171, -0.2952755905511810219 ) ) ;
#6216 = AXIS2_PLACEMENT_3D ( 'NONE', #3690, #2500, #4100 ) ;
#6217 = DIRECTION ( 'NONE',  ( -0.4724509005743147694, 0.8813569915457181159, -1.674621985683294870E-16 ) ) ;
#6218 = CARTESIAN_POINT ( 'NONE',  ( 0.3997746709170348356, 0.000000000000000000, 0.000000000000000000 ) ) ;
#6219 = CARTESIAN_POINT ( 'NONE',  ( 0.000000000000000000, 0.000000000000000000, 0.000000000000000000 ) ) ;
#6220 = AXIS2_PLACEMENT_3D ( 'NONE', #392, #6200, #3288 ) ;
#6221 = FACE_OUTER_BOUND ( 'NONE', #6009, .T. ) ;
#6222 = ADVANCED_FACE ( 'NONE', ( #1423 ), #1872, .F. ) ;
#6223 = EDGE_CURVE ( 'NONE', #2089, #4463, #3113, .T. ) ;
#6224 = EDGE_CURVE ( 'NONE', #6862, #5971, #716, .T. ) ;
#6225 = CARTESIAN_POINT ( 'NONE',  ( 0.4445641707282979582, 1.003668447264491226, -1.568529612473645862 ) ) ;
#6226 = AXIS2_PLACEMENT_3D ( 'NONE', #47, #5365, #6471 ) ;
#6227 = CARTESIAN_POINT ( 'NONE',  ( 3.198568410424924124, 2.407012729153881203, 0.4724409448818898127 ) ) ;
#6228 = CARTESIAN_POINT ( 'NONE',  ( 0.3442723180357430413, -0.1814473180894617399, 0.2762752072743029363 ) ) ;
#6229 = DIRECTION ( 'NONE',  ( -1.000000000000000000, -0.000000000000000000, -0.000000000000000000 ) ) ;
#6230 = CARTESIAN_POINT ( 'NONE',  ( -0.4445641707282975696, 1.003668447264491226, -1.568529612473645418 ) ) ;
#6231 = ORIENTED_EDGE ( 'NONE', *, *, #3704, .T. ) ;
#6232 = CARTESIAN_POINT ( 'NONE',  ( 0.05806029764938244742, -0.3756247315785402607, -0.3942118233966392382 ) ) ;
#6233 = ADVANCED_FACE ( 'NONE', ( #2471, #4269 ), #4807, .F. ) ;
#6234 = AXIS2_PLACEMENT_3D ( 'NONE', #6218, #3235, #977 ) ;
#6235 = ORIENTED_EDGE ( 'NONE', *, *, #5995, .F. ) ;
#6236 = CARTESIAN_POINT ( 'NONE',  ( 0.4685039370078740717, 0.1704774416898497680, -0.2952755905511810774 ) ) ;
#6237 = CARTESIAN_POINT ( 'NONE',  ( 0.3410249605999410294, 1.062103031354818709E-12, 0.3014927230551906479 ) ) ;
#6238 = CARTESIAN_POINT ( 'NONE',  ( -0.9773781006402562088, -0.4999740374263574871, -1.373989084484001477 ) ) ;
#6239 = ORIENTED_EDGE ( 'NONE', *, *, #4026, .F. ) ;
#6240 = CARTESIAN_POINT ( 'NONE',  ( 0.3388536909602617997, -0.2864058322153867353, 0.09448172812127884901 ) ) ;
#6241 = ORIENTED_EDGE ( 'NONE', *, *, #6926, .F. ) ;
#6242 = AXIS2_PLACEMENT_3D ( 'NONE', #2048, #6709, #3804 ) ;
#6243 = ORIENTED_EDGE ( 'NONE', *, *, #664, .F. ) ;
#6244 = CARTESIAN_POINT ( 'NONE',  ( 0.9971724964169936811, 0.4476001829033208201, -1.429776958199370451 ) ) ;
#6245 = SURFACE_SIDE_STYLE ('',( #5210 ) ) ;
#6246 = ORIENTED_EDGE ( 'NONE', *, *, #4664, .T. ) ;
#6247 = CARTESIAN_POINT ( 'NONE',  ( 0.000000000000000000, 1.496062992125984259, -0.7480314960629921295 ) ) ;
#6248 = ORIENTED_EDGE ( 'NONE', *, *, #4146, .F. ) ;
#6249 = VECTOR ( 'NONE', #7368, 39.37007874015748143 ) ;
#6250 = FACE_OUTER_BOUND ( 'NONE', #7119, .T. ) ;
#6251 = CARTESIAN_POINT ( 'NONE',  ( 0.3442723180356496160, 0.3299850069800976948, 0.01900038327686272982 ) ) ;
#6252 = ORIENTED_EDGE ( 'NONE', *, *, #134, .F. ) ;
#6253 = ORIENTED_EDGE ( 'NONE', *, *, #1588, .T. ) ;
#6254 = CARTESIAN_POINT ( 'NONE',  ( 0.3528999085283636150, -0.1454870853231272354, -0.3018102362147644380 ) ) ;
#6255 = DIRECTION ( 'NONE',  ( 0.000000000000000000, 0.000000000000000000, 1.000000000000000000 ) ) ;
#6256 = CIRCLE ( 'NONE', #5038, 0.2362204724409455170 ) ;
#6257 = CARTESIAN_POINT ( 'NONE',  ( -0.2948818897637794367, 3.611261624257350948E-17, 0.1188976377952756375 ) ) ;
#6258 = CARTESIAN_POINT ( 'NONE',  ( 0.8785537298370084125, 0.4700904924197999990, -1.433776001880364470 ) ) ;
#6259 = FILL_AREA_STYLE_COLOUR ( '', #6769 ) ;
#6260 = CIRCLE ( 'NONE', #2943, 0.9964144355006142595 ) ;
#6261 = CARTESIAN_POINT ( 'NONE',  ( 0.000000000000000000, 0.000000000000000000, 0.9842519685039370358 ) ) ;
#6262 =( CONVERSION_BASED_UNIT ( 'INCH', #2701 ) LENGTH_UNIT ( ) NAMED_UNIT ( #490 ) );
#6263 = TOROIDAL_SURFACE ( 'NONE', #5276, 1.124634398195722973, 0.05905511811023622659 ) ;
#6264 = EDGE_CURVE ( 'NONE', #96, #428, #749, .T. ) ;
#6265 = CARTESIAN_POINT ( 'NONE',  ( 0.2362204724409449341, 0.000000000000000000, 0.000000000000000000 ) ) ;
#6266 = CARTESIAN_POINT ( 'NONE',  ( 0.3387177083556423551, -0.2412911239081454440, 0.1726226950780508362 ) ) ;
#6267 = CYLINDRICAL_SURFACE ( 'NONE', #5890, 0.2362204724409455170 ) ;
#6268 = CARTESIAN_POINT ( 'NONE',  ( -1.702122929023921302E-15, 0.000000000000000000, -1.433776001880364026 ) ) ;
#6269 = AXIS2_PLACEMENT_3D ( 'NONE', #4959, #3776, #3736 ) ;
#6270 = EDGE_LOOP ( 'NONE', ( #699, #255, #2360, #1966 ) ) ;
#6271 = CARTESIAN_POINT ( 'NONE',  ( 0.000000000000000000, 0.000000000000000000, -1.515748031496062964 ) ) ;
#6272 = DIRECTION ( 'NONE',  ( 6.217248937900876626E-15, 1.000000000000000000, -2.256009703088257329E-15 ) ) ;
#6273 = EDGE_CURVE ( 'NONE', #3631, #5611, #3957, .T. ) ;
#6274 = CONTEXT_DEPENDENT_SHAPE_REPRESENTATION ( #2092, #5527 ) ;
#6275 = ADVANCED_FACE ( 'NONE', ( #7397 ), #3444, .T. ) ;
#6276 = DIRECTION ( 'NONE',  ( -1.000000000000000000, -0.000000000000000000, -4.625929269271482167E-15 ) ) ;
#6277 = ORIENTED_EDGE ( 'NONE', *, *, #4824, .T. ) ;
#6278 = CARTESIAN_POINT ( 'NONE',  ( 0.3479980290964227452, 0.3208941761715193852, -0.04760384692076755769 ) ) ;
#6279 = FACE_OUTER_BOUND ( 'NONE', #6847, .T. ) ;
#6280 = ORIENTED_EDGE ( 'NONE', *, *, #3092, .T. ) ;
#6281 = ORIENTED_EDGE ( 'NONE', *, *, #3981, .T. ) ;
#6282 = CARTESIAN_POINT ( 'NONE',  ( 1.212519938569362798, -0.06127190455375051276, 0.9823712398279822455 ) ) ;
#6283 = CARTESIAN_POINT ( 'NONE',  ( 0.000000000000000000, 1.496062992125984259, 0.7480314960629921295 ) ) ;
#6284 = B_SPLINE_CURVE_WITH_KNOTS ( 'NONE', 3,
 ( #7064, #4692, #1822, #1239, #3588, #1160 ),
 .UNSPECIFIED., .F., .F.,
 ( 4, 2, 4 ),
 ( 0.000000000000000000, 0.002233368740102886427, 0.004466737480205772853 ),
 .UNSPECIFIED. ) ;
#6285 = CARTESIAN_POINT ( 'NONE',  ( 0.000000000000000000, 0.000000000000000000, -1.484898342931014303 ) ) ;
#6286 = ORIENTED_EDGE ( 'NONE', *, *, #5949, .T. ) ;
#6287 = CARTESIAN_POINT ( 'NONE',  ( 0.3336175750056034617, -0.2841290694830839736, 0.09842519685039370636 ) ) ;
#6288 = ORIENTED_EDGE ( 'NONE', *, *, #6316, .T. ) ;
#6289 = CARTESIAN_POINT ( 'NONE',  ( -1.279527559055117836, 1.968503937007873850, 2.480314960629921295 ) ) ;
#6290 = CIRCLE ( 'NONE', #2976, 0.2362204724409449064 ) ;
#6291 = ORIENTED_EDGE ( 'NONE', *, *, #7513, .F. ) ;
#6292 = DIMENSIONAL_EXPONENTS ( 1.000000000000000000, 0.000000000000000000, 0.000000000000000000, 0.000000000000000000, 0.000000000000000000, 0.000000000000000000, 0.000000000000000000 ) ;
#6293 =( REPRESENTATION_RELATIONSHIP ('NONE','NONE', #303, #1307 ) REPRESENTATION_RELATIONSHIP_WITH_TRANSFORMATION ( #2180 )SHAPE_REPRESENTATION_RELATIONSHIP( ) );
#6294 = CARTESIAN_POINT ( 'NONE',  ( 0.5141614760841460852, -0.9609181420092316461, -1.361499588670819216 ) ) ;
#6295 = CARTESIAN_POINT ( 'NONE',  ( 18.41860179314716461, 41.48855051017370243, 54.38594198892901943 ) ) ;
#6296 = PLANE ( 'NONE',  #6352 ) ;
#6297 = CARTESIAN_POINT ( 'NONE',  ( 0.004822332172886236931, -0.2197023059474404461, 0.2100156246613535393 ) ) ;
#6298 = CARTESIAN_POINT ( 'NONE',  ( 0.8592737258235019215, 0.2005978551774719454, -0.9636033532647499955 ) ) ;
#6299 =( NAMED_UNIT ( * ) PLANE_ANGLE_UNIT ( ) SI_UNIT ( $, .RADIAN. ) );
#6300 =( BOUNDED_SURFACE ( )  B_SPLINE_SURFACE ( 3, 2, ( 
 ( #2426, #5424, #4760 ),
 ( #183, #1855, #5997 ),
 ( #3112, #4190, #6530 ),
 ( #1269, #6604, #2506 ),
 ( #3615, #5958, #2385 ),
 ( #7165, #5378, #712 ),
 ( #4719, #1311, #3659 ),
 ( #5461, #2348, #4683 ) ),
 .UNSPECIFIED., .F., .F., .F. ) 
 B_SPLINE_SURFACE_WITH_KNOTS ( ( 4, 2, 2, 4 ),
 ( 3, 3 ),
 ( 0.03551798592901340978, 0.03994769179990649566, 0.04216254473535303859, 0.04437739767079958153 ),
 ( 0.000000000000000000, 1.000000000000000000 ),
 .UNSPECIFIED. ) 
 GEOMETRIC_REPRESENTATION_ITEM ( )  RATIONAL_B_SPLINE_SURFACE ( (
 ( 1.000000000000000000, 0.8047781103519396906, 1.000000000000000000),
 ( 1.000000000000000000, 0.8123785826170297764, 1.000000000000000000),
 ( 1.000000000000000000, 0.8190671539034730664, 1.000000000000000000),
 ( 1.000000000000000000, 0.8191932076449999212, 1.000000000000000000),
 ( 1.000000000000000000, 0.8176085094066802839, 1.000000000000000000),
 ( 1.000000000000000000, 0.8122955484013585359, 1.000000000000000000),
 ( 1.000000000000000000, 0.8086308001281159452, 1.000000000000000000),
 ( 1.000000000000000000, 0.8047712537969721192, 1.000000000000000000) ) ) 
 REPRESENTATION_ITEM ( '' )  SURFACE ( )  );
#6301 = B_SPLINE_CURVE_WITH_KNOTS ( 'NONE', 3,
 ( #3666, #3818, #833, #5467, #3239, #1019, #7474, #58, #3535, #1229 ),
 .UNSPECIFIED., .F., .F.,
 ( 4, 2, 2, 2, 4 ),
 ( -7.765797721857259104E-06, 0.0005114169989440442345, 0.001030599795609945862, 0.001549782592275847273, 0.002068965388941748900 ),
 .UNSPECIFIED. ) ;
#6302 = DIRECTION ( 'NONE',  ( -1.000000000000000000, -0.000000000000000000, -0.000000000000000000 ) ) ;
#6303 = CARTESIAN_POINT ( 'NONE',  ( 0.3409812221349244332, -0.2467127425962881426, 0.1756638922268692060 ) ) ;
#6304 = DIRECTION ( 'NONE',  ( -0.000000000000000000, -0.000000000000000000, 1.000000000000000000 ) ) ;
#6305 = CARTESIAN_POINT ( 'NONE',  ( 0.02890955082422759503, -0.3924549231051219222, -0.3862566910637251216 ) ) ;
#6306 = EDGE_CURVE ( 'NONE', #3522, #2089, #5787, .T. ) ;
#6307 = ORIENTED_EDGE ( 'NONE', *, *, #1494, .T. ) ;
#6308 = AXIS2_PLACEMENT_3D ( 'NONE', #2165, #4498, #2202 ) ;
#6309 = CARTESIAN_POINT ( 'NONE',  ( -0.9044351468059373955, 0.4526810454163289199, -1.447629383090422772 ) ) ;
#6310 = CARTESIAN_POINT ( 'NONE',  ( 0.3410076799406688286, -0.2754140928391124454, -0.1259532371559686781 ) ) ;
#6311 = CARTESIAN_POINT ( 'NONE',  ( -0.4332839536939404601, -0.9726683636255534227, -1.452651081959920765 ) ) ;
#6312 = EDGE_LOOP ( 'NONE', ( #7264, #2575, #3641, #466 ) ) ;
#6313 = CARTESIAN_POINT ( 'NONE',  ( 0.000000000000000000, 0.000000000000000000, 0.000000000000000000 ) ) ;
#6314 = CARTESIAN_POINT ( 'NONE',  ( 0.3581828924050324825, -0.1743168766271116221, -0.3019256869348722061 ) ) ;
#6315 = EDGE_CURVE ( 'NONE', #4054, #2045, #35, .T. ) ;
#6316 = EDGE_CURVE ( 'NONE', #2154, #4786, #6493, .T. ) ;
#6317 = ORIENTED_EDGE ( 'NONE', *, *, #6966, .F. ) ;
#6318 = ADVANCED_BREP_SHAPE_REPRESENTATION ( '', ( #3913, #5166 ), #1726 ) ;
#6319 = CARTESIAN_POINT ( 'NONE',  ( 0.000000000000000000, 0.2559055118110236116, -0.4921259842519685179 ) ) ;
#6320 = EDGE_CURVE ( 'NONE', #5128, #6553, #2843, .T. ) ;
#6321 = DIRECTION ( 'NONE',  ( 0.000000000000000000, 0.000000000000000000, 1.000000000000000000 ) ) ;
#6322 = CARTESIAN_POINT ( 'NONE',  ( 0.9842519685039370358, 0.000000000000000000, -1.377952755905512028 ) ) ;
#6323 = ORIENTED_EDGE ( 'NONE', *, *, #2252, .T. ) ;
#6324 = CARTESIAN_POINT ( 'NONE',  ( 0.5141614760841457521, 0.000000000000000000, -2.204724409448820754 ) ) ;
#6325 = EDGE_LOOP ( 'NONE', ( #4322, #4084, #3574, #2527 ) ) ;
#6326 = CARTESIAN_POINT ( 'NONE',  ( 1.220472440944882164, 0.01566504975835071242, 0.9842519685039374799 ) ) ;
#6327 = ORIENTED_EDGE ( 'NONE', *, *, #4435, .T. ) ;
#6328 = CARTESIAN_POINT ( 'NONE',  ( 0.4685039370078740717, 0.000000000000000000, 0.000000000000000000 ) ) ;
#6329 = CARTESIAN_POINT ( 'NONE',  ( 33.78363125245377319, 38.11143353299877390, 51.90956403617312986 ) ) ;
#6330 = CARTESIAN_POINT ( 'NONE',  ( 0.1771653543307088463, -0.3068593950417300431, 7.886165872636028972E-17 ) ) ;
#6331 = SURFACE_SIDE_STYLE ('',( #559 ) ) ;
#6332 = CARTESIAN_POINT ( 'NONE',  ( 0.7499405322945513763, 0.03096673178975459240, -0.9837952645051013523 ) ) ;
#6333 = AXIS2_PLACEMENT_3D ( 'NONE', #3124, #231, #2552 ) ;
#6334 = FACE_OUTER_BOUND ( 'NONE', #853, .T. ) ;
#6335 = AXIS2_PLACEMENT_3D ( 'NONE', #3547, #1944, #761 ) ;
#6336 = DIRECTION ( 'NONE',  ( -1.000000000000000000, -0.000000000000000000, -0.000000000000000000 ) ) ;
#6337 = UNCERTAINTY_MEASURE_WITH_UNIT (LENGTH_MEASURE( 1.000000000000000082E-05 ), #4455, 'distance_accuracy_value', 'NONE');
#6338 = CARTESIAN_POINT ( 'NONE',  ( 0.1023119647485436629, -0.3500760196667498936, -0.4024809188492812773 ) ) ;
#6339 = TOROIDAL_SURFACE ( 'NONE', #5985, 1.043121362164705745, 0.05905511811023622659 ) ;
#6340 = CARTESIAN_POINT ( 'NONE',  ( 0.4514963146295077334, -0.9983958463931797978, -1.424958914991359960 ) ) ;
#6341 = CYLINDRICAL_SURFACE ( 'NONE', #6859, 0.9842519685039370358 ) ;
#6342 = CONTEXT_DEPENDENT_SHAPE_REPRESENTATION ( #6293, #4419 ) ;
#6343 = ADVANCED_FACE ( 'NONE', ( #7360 ), #2133, .F. ) ;
#6344 = CARTESIAN_POINT ( 'NONE',  ( -0.4377664870282949594, -0.9883299873891312481, -1.443420526770072598 ) ) ;
#6345 = ORIENTED_EDGE ( 'NONE', *, *, #2764, .F. ) ;
#6346 = DIRECTION ( 'NONE',  ( 0.000000000000000000, 1.000000000000000000, 2.256009703088257329E-15 ) ) ;
#6347 = AXIS2_PLACEMENT_3D ( 'NONE', #6257, #4500, #1014 ) ;
#6348 = CARTESIAN_POINT ( 'NONE',  ( 0.3496875272944827695, -0.1667004943313752652, 0.3018174552735723437 ) ) ;
#6349 = VERTEX_POINT ( 'NONE', #456 ) ;
#6350 = ORIENTED_EDGE ( 'NONE', *, *, #2117, .T. ) ;
#6351 = CARTESIAN_POINT ( 'NONE',  ( 0.000000000000000000, 0.2559055118110236116, -0.4921259842519685179 ) ) ;
#6352 = AXIS2_PLACEMENT_3D ( 'NONE', #6866, #1621, #2808 ) ;
#6353 = EDGE_CURVE ( 'NONE', #1333, #1455, #173, .T. ) ;
#6354 = CARTESIAN_POINT ( 'NONE',  ( 0.000000000000000000, 0.000000000000000000, 0.000000000000000000 ) ) ;
#6355 = EDGE_CURVE ( 'NONE', #4898, #5718, #5422, .T. ) ;
#6356 = CARTESIAN_POINT ( 'NONE',  ( 0.000000000000000000, 0.2559055118110236116, 0.000000000000000000 ) ) ;
#6357 = VERTEX_POINT ( 'NONE', #3851 ) ;
#6358 = CARTESIAN_POINT ( 'NONE',  ( 1.145762533245342940, 0.1725491722722915233, 0.9690247371578599722 ) ) ;
#6359 = CARTESIAN_POINT ( 'NONE',  ( -1.010073413237867923, 0.4416276115803053348, -1.570717210673254538 ) ) ;
#6360 = ADVANCED_FACE ( 'NONE', ( #6185, #2093, #1624 ), #3350, .F. ) ;
#6361 = ORIENTED_EDGE ( 'NONE', *, *, #986, .T. ) ;
#6362 = VERTEX_POINT ( 'NONE', #6261 ) ;
#6363 = CARTESIAN_POINT ( 'NONE',  ( 1.377952755905512028, 0.7480314960629921295, -0.7480314960629921295 ) ) ;
#6364 = DIRECTION ( 'NONE',  ( 0.000000000000000000, 0.000000000000000000, -1.000000000000000000 ) ) ;
#6365 = CIRCLE ( 'NONE', #3677, 0.05905511811023627516 ) ;
#6366 = ADVANCED_FACE ( 'NONE', ( #6221, #980, #7469 ), #5661, .F. ) ;
#6367 = DIRECTION ( 'NONE',  ( -0.000000000000000000, -0.000000000000000000, 1.000000000000000000 ) ) ;
#6368 = EDGE_CURVE ( 'NONE', #725, #6192, #7404, .T. ) ;
#6369 = FILL_AREA_STYLE ('',( #4004 ) ) ;
#6370 = CARTESIAN_POINT ( 'NONE',  ( -1.030265823844197293, -0.4349482548737299559, -1.574803149606299302 ) ) ;
#6371 = CIRCLE ( 'NONE', #6014, 0.7480314960629921295 ) ;
#6372 = CIRCLE ( 'NONE', #3068, 0.4724409448818896462 ) ;
#6373 = CARTESIAN_POINT ( 'NONE',  ( 0.3426404862726872280, -0.2318193597401798645, -0.2015595396344879719 ) ) ;
#6374 = CARTESIAN_POINT ( 'NONE',  ( 5.942930443104038687E-30, -1.702122929023921893E-15, -1.433776001880363582 ) ) ;
#6375 = DIRECTION ( 'NONE',  ( -1.000000000000000000, 0.000000000000000000, 0.000000000000000000 ) ) ;
#6376 = CIRCLE ( 'NONE', #6869, 0.2362204724409448231 ) ;
#6377 = CARTESIAN_POINT ( 'NONE',  ( 0.3483227611829846637, 0.1704774416898499345, 0.2952755905511810774 ) ) ;
#6378 = CARTESIAN_POINT ( 'NONE',  ( 0.3410425348215777031, -0.2462961272004795532, -0.1763890642357578975 ) ) ;
#6379 = CONTEXT_DEPENDENT_SHAPE_REPRESENTATION ( #6001, #5396 ) ;
#6380 = FACE_OUTER_BOUND ( 'NONE', #2674, .T. ) ;
#6381 = ORIENTED_EDGE ( 'NONE', *, *, #5103, .T. ) ;
#6382 = VECTOR ( 'NONE', #689, 39.37007874015748143 ) ;
#6383 = CARTESIAN_POINT ( 'NONE',  ( -0.9964144355006142595, 1.220255749060045517E-16, -1.433776001880363360 ) ) ;
#6384 = DIRECTION ( 'NONE',  ( 0.000000000000000000, -0.5000000000000012212, -0.8660254037844377084 ) ) ;
#6385 =( REPRESENTATION_RELATIONSHIP ('NONE','NONE', #303, #1307 ) REPRESENTATION_RELATIONSHIP_WITH_TRANSFORMATION ( #995 )SHAPE_REPRESENTATION_RELATIONSHIP( ) );
#6386 = CARTESIAN_POINT ( 'NONE',  ( 0.3465694189147047188, 0.3147628225698786419, 0.04536598007754604617 ) ) ;
#6387 = EDGE_LOOP ( 'NONE', ( #6549, #1224, #5438 ) ) ;
#6388 = ORIENTED_EDGE ( 'NONE', *, *, #5103, .F. ) ;
#6389 = DIRECTION ( 'NONE',  ( 0.000000000000000000, 0.000000000000000000, 1.000000000000000000 ) ) ;
#6390 = DIRECTION ( 'NONE',  ( 0.000000000000000000, 0.000000000000000000, -1.000000000000000000 ) ) ;
#6391 = EDGE_LOOP ( 'NONE', ( #2894, #3055, #878, #1127, #5642, #6158 ) ) ;
#6392 = CARTESIAN_POINT ( 'NONE',  ( -0.1922007978147441398, -0.2981786776988376020, -0.4082677165354330340 ) ) ;
#6393 = PLANE ( 'NONE',  #5856 ) ;
#6394 = ORIENTED_EDGE ( 'NONE', *, *, #5897, .T. ) ;
#6395 = AXIS2_PLACEMENT_3D ( 'NONE', #3390, #5771, #2779 ) ;
#6396 = EDGE_CURVE ( 'NONE', #5974, #1691, #3198, .T. ) ;
#6397 = CARTESIAN_POINT ( 'NONE',  ( 1.377952755905512028, 0.7480314960629921295, 0.7480314960629921295 ) ) ;
#6398 = DIRECTION ( 'NONE',  ( 0.000000000000000000, 0.000000000000000000, 1.000000000000000000 ) ) ;
#6399 = CARTESIAN_POINT ( 'NONE',  ( 1.056523642887408521, -0.5141614760841347609, -1.484898342931014303 ) ) ;
#6400 = CARTESIAN_POINT ( 'NONE',  ( -0.02890955082422807035, 0.3924549231051211451, -0.3862566910637255657 ) ) ;
#6401 = DIRECTION ( 'NONE',  ( 1.765631543889772066E-46, -1.000000000000000000, -2.207829878515936732E-15 ) ) ;
#6402 = ADVANCED_FACE ( 'NONE', ( #4426 ), #1016, .T. ) ;
#6403 = EDGE_CURVE ( 'NONE', #2762, #3843, #2750, .T. ) ;
#6404 =( NAMED_UNIT ( * ) SI_UNIT ( $, .STERADIAN. ) SOLID_ANGLE_UNIT ( ) );
#6405 = EDGE_CURVE ( 'NONE', #670, #4992, #1997, .T. ) ;
#6406 = DIRECTION ( 'NONE',  ( 1.000000000000000000, 0.000000000000000000, -0.000000000000000000 ) ) ;
#6407 = FACE_OUTER_BOUND ( 'NONE', #2687, .T. ) ;
#6408 = DIRECTION ( 'NONE',  ( -0.000000000000000000, -0.000000000000000000, -1.000000000000000000 ) ) ;
#6409 = DIRECTION ( 'NONE',  ( 0.000000000000000000, 1.000000000000000000, 0.000000000000000000 ) ) ;
#6410 = CARTESIAN_POINT ( 'NONE',  ( 0.4526814320286470794, -0.9044344578135156132, -1.447629106959917200 ) ) ;
#6411 = DIRECTION ( 'NONE',  ( 1.000000000000000000, 0.000000000000000000, 0.000000000000000000 ) ) ;
#6412 = CONTEXT_DEPENDENT_SHAPE_REPRESENTATION ( #536, #4355 ) ;
#6413 = DIRECTION ( 'NONE',  ( 0.000000000000000000, 0.000000000000000000, -1.000000000000000000 ) ) ;
#6414 = ORIENTED_EDGE ( 'NONE', *, *, #565, .T. ) ;
#6415 = CARTESIAN_POINT ( 'NONE',  ( -0.4837908950006660214, -1.080458485393811952, -1.514208454829283790 ) ) ;
#6416 = CARTESIAN_POINT ( 'NONE',  ( 0.000000000000000000, 0.000000000000000000, 0.000000000000000000 ) ) ;
#6417 = ORIENTED_EDGE ( 'NONE', *, *, #6396, .F. ) ;
#6418 = ORIENTED_EDGE ( 'NONE', *, *, #4155, .F. ) ;
#6419 = CARTESIAN_POINT ( 'NONE',  ( 0.3997746709170348356, 5.668966274263039413E-17, 0.4629062255509093782 ) ) ;
#6420 = DIRECTION ( 'NONE',  ( 1.000000000000000000, 0.000000000000000000, 0.000000000000000000 ) ) ;
#6421 =( REPRESENTATION_RELATIONSHIP ('NONE','NONE', #303, #5265 ) REPRESENTATION_RELATIONSHIP_WITH_TRANSFORMATION ( #4117 )SHAPE_REPRESENTATION_RELATIONSHIP( ) );
#6422 = CARTESIAN_POINT ( 'NONE',  ( 0.3410249605999410294, -1.062517223525361548E-12, -0.3014927230551905368 ) ) ;
#6423 = VERTEX_POINT ( 'NONE', #4642 ) ;
#6424 = CARTESIAN_POINT ( 'NONE',  ( -2.834645669291338432, 0.000000000000000000, 0.000000000000000000 ) ) ;
#6425 = FACE_OUTER_BOUND ( 'NONE', #463, .T. ) ;
#6426 = FACE_OUTER_BOUND ( 'NONE', #5031, .T. ) ;
#6427 = ORIENTED_EDGE ( 'NONE', *, *, #1496, .F. ) ;
#6428 = ORIENTED_EDGE ( 'NONE', *, *, #1767, .F. ) ;
#6429 = CARTESIAN_POINT ( 'NONE',  ( -1.782879132931211256E-29, 1.702122929023921696E-15, -1.433776001880364026 ) ) ;
#6430 = CARTESIAN_POINT ( 'NONE',  ( 33.78363125245377319, 38.11143353299877390, 54.79420970546446767 ) ) ;
#6431 = DIRECTION ( 'NONE',  ( -0.000000000000000000, -0.000000000000000000, 1.000000000000000000 ) ) ;
#6432 = CARTESIAN_POINT ( 'NONE',  ( 1.968503937007874072, 0.000000000000000000, 0.000000000000000000 ) ) ;
#6433 = ORIENTED_EDGE ( 'NONE', *, *, #3794, .F. ) ;
#6434 = CARTESIAN_POINT ( 'NONE',  ( -1.085572738833919360, -0.4589124540220979043, -1.540322878613942903 ) ) ;
#6435 = CONICAL_SURFACE ( 'NONE', #3142, 0.1982677165354330695, 0.7853981633974452814 ) ;
#6436 = ADVANCED_FACE ( 'NONE', ( #19 ), #5332, .T. ) ;
#6437 = DIRECTION ( 'NONE',  ( 1.000000000000000000, 0.000000000000000000, -0.000000000000000000 ) ) ;
#6438 = DIRECTION ( 'NONE',  ( 0.000000000000000000, 0.000000000000000000, 1.000000000000000000 ) ) ;
#6439 = ORIENTED_EDGE ( 'NONE', *, *, #5018, .T. ) ;
#6440 = AXIS2_PLACEMENT_3D ( 'NONE', #6652, #7138, #3047 ) ;
#6441 = CARTESIAN_POINT ( 'NONE',  ( 7.874015748031496287, 0.000000000000000000, 0.000000000000000000 ) ) ;
#6442 = PLANE ( 'NONE',  #1718 ) ;
#6443 =( NAMED_UNIT ( * ) SI_UNIT ( $, .STERADIAN. ) SOLID_ANGLE_UNIT ( ) );
#6444 = ADVANCED_FACE ( 'NONE', ( #7012, #1117 ), #1763, .T. ) ;
#6445 = DIRECTION ( 'NONE',  ( -0.000000000000000000, -0.000000000000000000, 1.000000000000000000 ) ) ;
#6446 = EDGE_CURVE ( 'NONE', #6705, #5707, #24, .T. ) ;
#6447 = CARTESIAN_POINT ( 'NONE',  ( 0.3426148638729746843, -0.05855635169929876427, -0.3015406112749626777 ) ) ;
#6448 = ADVANCED_FACE ( 'NONE', ( #93 ), #4052, .T. ) ;
#6449 = DIRECTION ( 'NONE',  ( -1.000000000000000000, 0.000000000000000000, 0.000000000000000000 ) ) ;
#6450 = CARTESIAN_POINT ( 'NONE',  ( 0.3543307086614173040, -0.03456946083495021638, 4.441920810010739880E-17 ) ) ;
#6451 = CARTESIAN_POINT ( 'NONE',  ( 0.3483227611829846637, 0.1704774416898499345, 0.2952755905511810774 ) ) ;
#6452 = VECTOR ( 'NONE', #7347, 39.37007874015748143 ) ;
#6453 = CARTESIAN_POINT ( 'NONE',  ( -1.729881963583410815E-29, 1.651526287078852914E-15, -1.456692913385827515 ) ) ;
#6454 = ADVANCED_FACE ( 'NONE', ( #4713 ), #1802, .F. ) ;
#6455 = VERTEX_POINT ( 'NONE', #4758 ) ;
#6456 = CARTESIAN_POINT ( 'NONE',  ( -0.4755998196564488745, -1.083679103503828456, -1.522578840002906997 ) ) ;
#6457 = DIRECTION ( 'NONE',  ( -0.000000000000000000, -0.000000000000000000, 1.000000000000000000 ) ) ;
#6458 = AXIS2_PLACEMENT_3D ( 'NONE', #5668, #3166, #423 ) ;
#6459 = ORIENTED_EDGE ( 'NONE', *, *, #2887, .F. ) ;
#6460 = ORIENTED_EDGE ( 'NONE', *, *, #571, .T. ) ;
#6461 = CARTESIAN_POINT ( 'NONE',  ( 0.3410249605999788325, 0.02903799983316233957, 0.3014927230551917026 ) ) ;
#6462 = AXIS2_PLACEMENT_3D ( 'NONE', #1197, #1864, #5963 ) ;
#6463 = FACE_OUTER_BOUND ( 'NONE', #4792, .T. ) ;
#6464 = EDGE_LOOP ( 'NONE', ( #2669, #2991, #3344, #3640 ) ) ;
#6465 = DIRECTION ( 'NONE',  ( 0.000000000000000000, -1.001543065824774208E-16, -1.000000000000000000 ) ) ;
#6466 = CARTESIAN_POINT ( 'NONE',  ( -0.7480314960629922405, 1.220472440944881942, 0.4724409448818898127 ) ) ;
#6467 = CARTESIAN_POINT ( 'NONE',  ( 0.000000000000000000, 0.2559055118110236116, 0.4921259842519685179 ) ) ;
#6468 = ORIENTED_EDGE ( 'NONE', *, *, #793, .F. ) ;
#6469 = CIRCLE ( 'NONE', #257, 0.7480314960629921295 ) ;
#6470 = DIRECTION ( 'NONE',  ( 0.000000000000000000, 1.000000000000000000, -2.193342766891360832E-15 ) ) ;
#6471 = DIRECTION ( 'NONE',  ( 1.000000000000000000, 1.045898529308442724E-14, 0.000000000000000000 ) ) ;
#6472 = CARTESIAN_POINT ( 'NONE',  ( 26.63278072698489041, 34.81515369617523703, 53.04224120152746025 ) ) ;
#6473 =( NAMED_UNIT ( * ) SI_UNIT ( $, .STERADIAN. ) SOLID_ANGLE_UNIT ( ) );
#6474 = B_SPLINE_CURVE_WITH_KNOTS ( 'NONE', 3,
 ( #4121, #36, #1873, #5933, #73, #573, #2358, #3591, #2319, #2972, #5972, #2444, #6456, #6415, #4085, #3511, #1054, #116 ),
 .UNSPECIFIED., .F., .F.,
 ( 4, 2, 2, 2, 2, 2, 2, 2, 4 ),
 ( 0.000000000000000000, 0.0002327816859446661863, 0.0004655633718893323727, 0.0009311267437786552043, 0.001396690115667977928, 0.001862253487557300868, 0.002327816859446623591, 0.002793380231335946314, 0.003724506975114578750 ),
 .UNSPECIFIED. ) ;
#6475 = CARTESIAN_POINT ( 'NONE',  ( 0.3337350301074833991, 0.05917206666036364110, 0.2952755905511810774 ) ) ;
#6476 = ORIENTED_EDGE ( 'NONE', *, *, #4447, .T. ) ;
#6477 = CARTESIAN_POINT ( 'NONE',  ( -1.084813395429186977, -0.4713813068963941810, -1.526966363676887095 ) ) ;
#6478 = ORIENTED_EDGE ( 'NONE', *, *, #160, .T. ) ;
#6479 = CARTESIAN_POINT ( 'NONE',  ( 0.000000000000000000, 0.3409548833797004797, 2.164902785881980513E-17 ) ) ;
#6480 = CARTESIAN_POINT ( 'NONE',  ( -1.037563309807723488, -0.4338950423154175340, -1.574803149606299302 ) ) ;
#6481 = ORIENTED_EDGE ( 'NONE', *, *, #4073, .T. ) ;
#6482 = CIRCLE ( 'NONE', #6242, 0.2362204724409449896 ) ;
#6483 = PRODUCT_DEFINITION_SHAPE ( 'NONE', 'NONE',  #7544 ) ;
#6484 = DIRECTION ( 'NONE',  ( 0.000000000000000000, 0.000000000000000000, -1.000000000000000000 ) ) ;
#6485 = CARTESIAN_POINT ( 'NONE',  ( 1.041228047528450995, 0.4333661275892136122, -1.574803149606299302 ) ) ;
#6486 = DIRECTION ( 'NONE',  ( 0.000000000000000000, -1.224646799147353700E-16, 1.000000000000000000 ) ) ;
#6487 = CARTESIAN_POINT ( 'NONE',  ( 0.000000000000000000, 1.496062992125984259, 0.000000000000000000 ) ) ;
#6488 = AXIS2_PLACEMENT_3D ( 'NONE', #1898, #636, #4229 ) ;
#6489 = CARTESIAN_POINT ( 'NONE',  ( 0.3337358785015786533, -0.05918271685993679171, -0.2952755905511810774 ) ) ;
#6490 = B_SPLINE_CURVE_WITH_KNOTS ( 'NONE', 3,
 ( #4510, #3900, #6762, #3320, #5669, #4008 ),
 .UNSPECIFIED., .F., .F.,
 ( 4, 2, 4 ),
 ( 0.007897041933671775787, 0.01008815886328916570, 0.01227927579290655560 ),
 .UNSPECIFIED. ) ;
#6491 = CARTESIAN_POINT ( 'NONE',  ( 0.4762522394722484842, -0.9941399105654876722, -1.397361772547373260 ) ) ;
#6492 = EDGE_CURVE ( 'NONE', #1409, #2214, #4424, .T. ) ;
#6493 = CIRCLE ( 'NONE', #3462, 0.2362204724409455170 ) ;
#6494 = CARTESIAN_POINT ( 'NONE',  ( 0.3543307086614173596, -0.1713008003332313067, -0.02204270589528177851 ) ) ;
#6495 = CARTESIAN_POINT ( 'NONE',  ( 0.5141614760841459741, -1.056523642887403192, -1.484898342931014303 ) ) ;
#6496 = CONTEXT_DEPENDENT_SHAPE_REPRESENTATION ( #4580, #941 ) ;
#6497 = CARTESIAN_POINT ( 'NONE',  ( 1.083410700381141289, 0.4508657589754813122, -1.549345605342071552 ) ) ;
#6498 = AXIS2_PLACEMENT_3D ( 'NONE', #2446, #6059, #3556 ) ;
#6499 = FACE_OUTER_BOUND ( 'NONE', #4063, .T. ) ;
#6500 = DIRECTION ( 'NONE',  ( -0.000000000000000000, -0.000000000000000000, -1.000000000000000000 ) ) ;
#6501 = CARTESIAN_POINT ( 'NONE',  ( -0.7480314960629922405, 1.220472440944881942, 2.480314960629921295 ) ) ;
#6502 = ORIENTED_EDGE ( 'NONE', *, *, #6543, .F. ) ;
#6503 = DIRECTION ( 'NONE',  ( -1.000000000000000000, 0.000000000000000000, 0.000000000000000000 ) ) ;
#6504 = DIRECTION ( 'NONE',  ( 1.000000000000000000, 0.000000000000000000, 0.000000000000000000 ) ) ;
#6505 = CIRCLE ( 'NONE', #2231, 0.4921259842519685179 ) ;
#6506 = EDGE_LOOP ( 'NONE', ( #6595, #6246, #1306, #1203, #3250, #5395 ) ) ;
#6507 = EDGE_CURVE ( 'NONE', #1455, #1333, #756, .T. ) ;
#6508 = VERTEX_POINT ( 'NONE', #4036 ) ;
#6509 = ADVANCED_FACE ( 'NONE', ( #3573 ), #1725, .T. ) ;
#6510 = FACE_OUTER_BOUND ( 'NONE', #2516, .T. ) ;
#6511 = ADVANCED_BREP_SHAPE_REPRESENTATION ( '', ( #6665, #5166 ), #4787 ) ;
#6512 = CONICAL_SURFACE ( 'NONE', #770, 0.3543307086614173596, 1.047197551196596521 ) ;
#6513 = CARTESIAN_POINT ( 'NONE',  ( 0.3485777078273625817, 0.3195689143662219234, -0.04989192643193119531 ) ) ;
#6514 = ORIENTED_EDGE ( 'NONE', *, *, #4351, .T. ) ;
#6515 = CARTESIAN_POINT ( 'NONE',  ( 0.4762527114670027650, 0.9941396836775473478, -1.397361282224857781 ) ) ;
#6516 = EDGE_LOOP ( 'NONE', ( #1287, #2801, #2200, #3187 ) ) ;
#6517 = AXIS2_PLACEMENT_3D ( 'NONE', #2853, #7508, #4614 ) ;
#6518 = ORIENTED_EDGE ( 'NONE', *, *, #2480, .F. ) ;
#6519 = FACE_OUTER_BOUND ( 'NONE', #4693, .T. ) ;
#6520 = SHAPE_DEFINITION_REPRESENTATION ( #2641, #5265 ) ;
#6521 =( CONVERSION_BASED_UNIT ( 'INCH', #2416 ) LENGTH_UNIT ( ) NAMED_UNIT ( #1012 ) );
#6522 = CARTESIAN_POINT ( 'NONE',  ( 0.3531509790457915132, 0.1471070558423459573, 0.3018164037399326816 ) ) ;
#6523 = CARTESIAN_POINT ( 'NONE',  ( 0.3483227611829846082, 0.1704774416898497680, -0.2952755905511810774 ) ) ;
#6524 = ORIENTED_EDGE ( 'NONE', *, *, #287, .T. ) ;
#6525 = CARTESIAN_POINT ( 'NONE',  ( 0.000000000000000000, 0.2557161625347749712, -0.1476377952755909551 ) ) ;
#6526 = ORIENTED_EDGE ( 'NONE', *, *, #4588, .T. ) ;
#6527 =( NAMED_UNIT ( * ) SI_UNIT ( $, .STERADIAN. ) SOLID_ANGLE_UNIT ( ) );
#6528 = CLOSED_SHELL ( 'NONE', ( #615, #794, #2806, #652, #6366, #7057, #2846, #3078, #3785, #2280, #2022, #3649 ) ) ;
#6529 = CYLINDRICAL_SURFACE ( 'NONE', #2706, 0.3543307086614172485 ) ;
#6530 = CARTESIAN_POINT ( 'NONE',  ( 0.3411151615605753085, -0.2304996462388200218, -0.2037536041052529223 ) ) ;
#6531 = DIRECTION ( 'NONE',  ( -2.207829878515936732E-15, 0.000000000000000000, 1.000000000000000000 ) ) ;
#6532 = DIRECTION ( 'NONE',  ( -0.000000000000000000, -0.000000000000000000, 1.000000000000000000 ) ) ;
#6533 =( REPRESENTATION_RELATIONSHIP ('NONE','NONE', #303, #5265 ) REPRESENTATION_RELATIONSHIP_WITH_TRANSFORMATION ( #1905 )SHAPE_REPRESENTATION_RELATIONSHIP( ) );
#6534 = CARTESIAN_POINT ( 'NONE',  ( -0.4416272204090970765, -1.010074371201533205, -1.570717485485533249 ) ) ;
#6535 = CARTESIAN_POINT ( 'NONE',  ( 0.9726684123052288244, 0.4332839571663439915, -1.452651065350217596 ) ) ;
#6536 = DIRECTION ( 'NONE',  ( -1.000000000000000000, 0.000000000000000000, -0.000000000000000000 ) ) ;
#6537 = CARTESIAN_POINT ( 'NONE',  ( 0.3483227611829848303, -0.1704774416898505729, -0.2952755905511810774 ) ) ;
#6538 = PLANE ( 'NONE',  #4613 ) ;
#6539 = FACE_OUTER_BOUND ( 'NONE', #4564, .T. ) ;
#6540 = MANIFOLD_SOLID_BREP ( 'TorqueElement', #305 ) ;
#6541 = ORIENTED_EDGE ( 'NONE', *, *, #4017, .T. ) ;
#6542 = CARTESIAN_POINT ( 'NONE',  ( 3.198568410424924124, 2.407012729153881203, 0.000000000000000000 ) ) ;
#6543 = EDGE_CURVE ( 'NONE', #1419, #1683, #1088, .T. ) ;
#6544 = DIRECTION ( 'NONE',  ( 7.708596820178695308E-30, -2.207829878515936732E-15, 1.000000000000000000 ) ) ;
#6545 = VERTEX_POINT ( 'NONE', #7127 ) ;
#6546 = FACE_BOUND ( 'NONE', #634, .T. ) ;
#6547 = FACE_OUTER_BOUND ( 'NONE', #491, .T. ) ;
#6548 = DIRECTION ( 'NONE',  ( -0.000000000000000000, -0.000000000000000000, 1.000000000000000000 ) ) ;
#6549 = ORIENTED_EDGE ( 'NONE', *, *, #2492, .T. ) ;
#6550 = CARTESIAN_POINT ( 'NONE',  ( 0.4596436929058889120, 0.9990286721055788854, -1.415369458146013226 ) ) ;
#6551 = EDGE_CURVE ( 'NONE', #662, #3879, #6727, .T. ) ;
#6552 = EDGE_CURVE ( 'NONE', #5853, #5110, #262, .T. ) ;
#6553 = VERTEX_POINT ( 'NONE', #4914 ) ;
#6554 = PRODUCT_DEFINITION_SHAPE ( 'NONE', 'NONE',  #7524 ) ;
#6555 = ORIENTED_EDGE ( 'NONE', *, *, #7387, .F. ) ;
#6556 = EDGE_CURVE ( 'NONE', #3765, #4054, #3545, .T. ) ;
#6557 = CARTESIAN_POINT ( 'NONE',  ( 0.3337354549119980751, -0.2853048623713481113, -0.09638866382874244909 ) ) ;
#6558 = PRODUCT_DEFINITION_FORMATION_WITH_SPECIFIED_SOURCE ( 'ANY', '', #5321, .NOT_KNOWN. ) ;
#6559 = CARTESIAN_POINT ( 'NONE',  ( -0.3253487914207031650, 0.2213056477483777706, -0.3862808132025623009 ) ) ;
#6560 = APPLICATION_PROTOCOL_DEFINITION ( 'draft international standard', 'automotive_design', 1998, #3004 ) ;
#6561 = DIRECTION ( 'NONE',  ( 0.000000000000000000, 0.000000000000000000, -1.000000000000000000 ) ) ;
#6562 = CARTESIAN_POINT ( 'NONE',  ( -1.056523642887401415, -0.5141614760841493048, -1.484898342931014303 ) ) ;
#6563 = CARTESIAN_POINT ( 'NONE',  ( -0.4526814320286470794, -0.9044344578135171675, -1.447629106959918754 ) ) ;
#6564 = ORIENTED_EDGE ( 'NONE', *, *, #1576, .F. ) ;
#6565 = CARTESIAN_POINT ( 'NONE',  ( 1.220472440944881720, -1.984939871850715226E-17, 0.9842519685039370358 ) ) ;
#6566 = DIRECTION ( 'NONE',  ( 0.000000000000000000, 0.000000000000000000, 1.000000000000000000 ) ) ;
#6567 = ORIENTED_EDGE ( 'NONE', *, *, #5061, .T. ) ;
#6568 = CARTESIAN_POINT ( 'NONE',  ( 0.000000000000000000, 1.496062992125984259, 0.000000000000000000 ) ) ;
#6569 = CARTESIAN_POINT ( 'NONE',  ( 0.4508656291625806056, -1.083410641227605664, -1.549345754620972127 ) ) ;
#6570 = AXIS2_PLACEMENT_3D ( 'NONE', #2898, #6548, #40 ) ;
#6571 = CARTESIAN_POINT ( 'NONE',  ( -0.9666437042230142662, 0.4330708661417289052, -1.454455828411335583 ) ) ;
#6572 = DIRECTION ( 'NONE',  ( 0.000000000000000000, 0.000000000000000000, -1.000000000000000000 ) ) ;
#6573 = LINE ( 'NONE', #5468, #5493 ) ;
#6574 = CARTESIAN_POINT ( 'NONE',  ( 0.3483227611829849413, -0.3409548833797009237, 0.000000000000000000 ) ) ;
#6575 = DIRECTION ( 'NONE',  ( -2.207829878515936732E-15, 0.000000000000000000, 1.000000000000000000 ) ) ;
#6576 = CARTESIAN_POINT ( 'NONE',  ( 5.154746071126671174E-15, -0.4921259842519683514, -2.204724409448820754 ) ) ;
#6577 = CARTESIAN_POINT ( 'NONE',  ( 0.01168997831664858947, 0.1984671517595417711, 0.2467959906213527677 ) ) ;
#6578 = EDGE_LOOP ( 'NONE', ( #5463, #5746 ) ) ;
#6579 = CARTESIAN_POINT ( 'NONE',  ( -0.9941399105654891155, 0.4762522394722451535, -1.397361772547373038 ) ) ;
#6580 = DIRECTION ( 'NONE',  ( -0.000000000000000000, -0.000000000000000000, 1.000000000000000000 ) ) ;
#6581 = VERTEX_POINT ( 'NONE', #5992 ) ;
#6582 = CIRCLE ( 'NONE', #2415, 0.4921259842519685179 ) ;
#6583 = CARTESIAN_POINT ( 'NONE',  ( 0.4330708661417321803, 1.051607560569805422, -1.573502278225820339 ) ) ;
#6584 = ORIENTED_EDGE ( 'NONE', *, *, #5010, .T. ) ;
#6585 = AXIS2_PLACEMENT_3D ( 'NONE', #7174, #4847, #6614 ) ;
#6586 = CARTESIAN_POINT ( 'NONE',  ( 0.5073702590884642261, 0.9696319393317771596, -1.367288630522805359 ) ) ;
#6587 = EDGE_LOOP ( 'NONE', ( #2078, #927, #7415, #3798, #6103, #2994, #3859, #2010 ) ) ;
#6588 = VERTEX_POINT ( 'NONE', #6565 ) ;
#6589 = DIRECTION ( 'NONE',  ( 1.000000000000000000, 0.000000000000000000, 0.000000000000000000 ) ) ;
#6590 = AXIS2_PLACEMENT_3D ( 'NONE', #5213, #2870, #4668 ) ;
#6591 = EDGE_CURVE ( 'NONE', #4474, #1329, #6365, .T. ) ;
#6592 = ADVANCED_FACE ( 'NONE', ( #862 ), #1213, .T. ) ;
#6593 = CONTEXT_DEPENDENT_SHAPE_REPRESENTATION ( #5216, #2039 ) ;
#6594 = PRESENTATION_STYLE_ASSIGNMENT (( #5327 ) ) ;
#6595 = ORIENTED_EDGE ( 'NONE', *, *, #5479, .T. ) ;
#6596 = CARTESIAN_POINT ( 'NONE',  ( 0.3585665266928871331, 0.1764011776056260972, 0.3019340455778471433 ) ) ;
#6597 = ORIENTED_EDGE ( 'NONE', *, *, #298, .F. ) ;
#6598 = ADVANCED_FACE ( 'NONE', ( #4876 ), #2012, .F. ) ;
#6599 = AXIS2_PLACEMENT_3D ( 'NONE', #2017, #6679, #3888 ) ;
#6600 = CARTESIAN_POINT ( 'NONE',  ( 0.3585569128062318645, 0.1733077889112127901, 0.3036897776982951380 ) ) ;
#6601 = ORIENTED_EDGE ( 'NONE', *, *, #4289, .T. ) ;
#6602 = EDGE_CURVE ( 'NONE', #2406, #3362, #4771, .T. ) ;
#6603 = EDGE_CURVE ( 'NONE', #2461, #4570, #6763, .T. ) ;
#6604 = CARTESIAN_POINT ( 'NONE',  ( 0.3387177083556159873, -0.2701412011614057196, -0.1226528954731239129 ) ) ;
#6605 = LINE ( 'NONE', #101, #5064 ) ;
#6606 = CARTESIAN_POINT ( 'NONE',  ( 0.4755998196564493741, -1.083679103503828456, -1.522578840002907219 ) ) ;
#6607 = COLOUR_RGB ( '',0.7921568627450980005, 0.8196078431372548767, 0.9333333333333333481 ) ;
#6608 = CARTESIAN_POINT ( 'NONE',  ( 0.01178921041716498620, 0.1149842948508797008, -0.2952755905511810774 ) ) ;
#6609 = CARTESIAN_POINT ( 'NONE',  ( 0.02898191724071416675, 0.3924131423350827874, -0.02198690333287090654 ) ) ;
#6610 = CARTESIAN_POINT ( 'NONE',  ( 1.051607560569801425, 0.4330708661417428385, -1.573502278225820783 ) ) ;
#6611 = CIRCLE ( 'NONE', #3313, 0.4921259842519685179 ) ;
#6612 = CARTESIAN_POINT ( 'NONE',  ( 0.01178921041716498620, 0.1149842948508797008, -0.2952755905511810774 ) ) ;
#6613 = CARTESIAN_POINT ( 'NONE',  ( -0.1771653543307088186, -0.3068593950417299876, 7.886165872636028972E-17 ) ) ;
#6614 = DIRECTION ( 'NONE',  ( 1.000000000000000000, 0.000000000000000000, 0.000000000000000000 ) ) ;
#6615 = CARTESIAN_POINT ( 'NONE',  ( 1.649606299212598381, 2.660472849486257786E-17, -0.1982677165354330695 ) ) ;
#6616 = ORIENTED_EDGE ( 'NONE', *, *, #6784, .F. ) ;
#6617 = PRODUCT_DEFINITION_SHAPE ( 'NONE', 'NONE',  #7548 ) ;
#6618 = LINE ( 'NONE', #1990, #4671 ) ;
#6619 = CARTESIAN_POINT ( 'NONE',  ( -0.4368170150760394277, 0.9411660957780404457, -1.456692913385828847 ) ) ;
#6620 = ORIENTED_EDGE ( 'NONE', *, *, #4764, .T. ) ;
#6621 = AXIS2_PLACEMENT_3D ( 'NONE', #2807, #3265, #6255 ) ;
#6622 = SPHERICAL_SURFACE ( 'NONE', #2097, 1.377952755905511806 ) ;
#6623 = AXIS2_PLACEMENT_3D ( 'NONE', #7266, #6169, #5530 ) ;
#6624 = DIRECTION ( 'NONE',  ( -1.000000000000000000, -0.000000000000000000, -0.000000000000000000 ) ) ;
#6625 = CARTESIAN_POINT ( 'NONE',  ( 0.002513486811083733702, -0.2268523693227597338, -0.1976313516179637741 ) ) ;
#6626 = AXIS2_PLACEMENT_3D ( 'NONE', #4072, #3496, #1225 ) ;
#6627 = ORIENTED_EDGE ( 'NONE', *, *, #6913, .T. ) ;
#6628 = CARTESIAN_POINT ( 'NONE',  ( 0.3388536909602617997, 0.2864058322153591463, -0.09448172812127442199 ) ) ;
#6629 = VERTEX_POINT ( 'NONE', #6525 ) ;
#6630 = AXIS2_PLACEMENT_3D ( 'NONE', #1630, #3940, #6882 ) ;
#6631 = DIRECTION ( 'NONE',  ( -0.000000000000000000, -0.000000000000000000, 1.000000000000000000 ) ) ;
#6632 = VECTOR ( 'NONE', #342, 39.37007874015748143 ) ;
#6633 = SURFACE_STYLE_USAGE ( .BOTH. , #6738 ) ;
#6634 = CARTESIAN_POINT ( 'NONE',  ( 0.3479980290963966549, 0.2016732288369792181, 0.2541005850305664282 ) ) ;
#6635 = ORIENTED_EDGE ( 'NONE', *, *, #160, .F. ) ;
#6636 = CARTESIAN_POINT ( 'NONE',  ( 1.121892893784558254, 0.1921327968434894951, 0.9653269806155788668 ) ) ;
#6637 = AXIS2_PLACEMENT_3D ( 'NONE', #7177, #3243, #5592 ) ;
#6638 = CARTESIAN_POINT ( 'NONE',  ( 0.3528971332113848836, -0.3341112492250008503, 0.02492269209175877395 ) ) ;
#6639 = EDGE_CURVE ( 'NONE', #7450, #161, #1386, .T. ) ;
#6640 = EDGE_LOOP ( 'NONE', ( #7085, #4492 ) ) ;
#6641 = CARTESIAN_POINT ( 'NONE',  ( 3.414809992080329023E-17, 0.4091458600556405201, -0.3766201741223081378 ) ) ;
#6642 = CARTESIAN_POINT ( 'NONE',  ( 1.212838072735738848, -0.06155971505712520137, -0.9824432156515408021 ) ) ;
#6643 = VECTOR ( 'NONE', #5122, 39.37007874015748143 ) ;
#6644 = CARTESIAN_POINT ( 'NONE',  ( 0.4375700189966303388, -1.070856827570678904, -1.565644132322242532 ) ) ;
#6645 = EDGE_CURVE ( 'NONE', #614, #931, #3057, .T. ) ;
#6646 = ADVANCED_FACE ( 'NONE', ( #4834 ), #4454, .F. ) ;
#6647 = DIRECTION ( 'NONE',  ( 1.000000000000000000, 0.000000000000000000, -0.000000000000000000 ) ) ;
#6648 = CARTESIAN_POINT ( 'NONE',  ( 0.7480314960629922405, 1.220472440944881942, 2.480314960629921295 ) ) ;
#6649 = B_SPLINE_CURVE_WITH_KNOTS ( 'NONE', 3,
 ( #7223, #6729, #1998, #4329 ),
 .UNSPECIFIED., .F., .F.,
 ( 4, 4 ),
 ( 3.469446951953614189E-18, 0.0004815725036528502637 ),
 .UNSPECIFIED. ) ;
#6650 = CYLINDRICAL_SURFACE ( 'NONE', #720, 0.4921259842519685179 ) ;
#6651 = FACE_OUTER_BOUND ( 'NONE', #4219, .T. ) ;
#6652 = CARTESIAN_POINT ( 'NONE',  ( 0.000000000000000000, 0.000000000000000000, 0.000000000000000000 ) ) ;
#6653 = DIRECTION ( 'NONE',  ( 0.000000000000000000, -1.000000000000000000, 0.000000000000000000 ) ) ;
#6654 = CARTESIAN_POINT ( 'NONE',  ( 0.7480314960629922405, 1.220472440944881942, 0.000000000000000000 ) ) ;
#6655 = ORIENTED_EDGE ( 'NONE', *, *, #6224, .T. ) ;
#6656 = VECTOR ( 'NONE', #4842, 39.37007874015748143 ) ;
#6657 = FACE_OUTER_BOUND ( 'NONE', #311, .T. ) ;
#6658 = CARTESIAN_POINT ( 'NONE',  ( -0.4403525121893726579, 1.075170037517933386, -1.561970602951606280 ) ) ;
#6659 = EDGE_LOOP ( 'NONE', ( #4604, #92, #1830, #4530 ) ) ;
#6660 = DIRECTION ( 'NONE',  ( 0.000000000000000000, 1.000000000000000000, 0.000000000000000000 ) ) ;
#6661 = CARTESIAN_POINT ( 'NONE',  ( -1.320571051624814422E-17, -0.02882762270237488114, -0.2952755905511810219 ) ) ;
#6662 = DIRECTION ( 'NONE',  ( -1.000000000000000000, -0.000000000000000000, -0.000000000000000000 ) ) ;
#6663 = ORIENTED_EDGE ( 'NONE', *, *, #1302, .F. ) ;
#6664 = CARTESIAN_POINT ( 'NONE',  ( 1.968503937007874072, 1.496062992125984259, 0.000000000000000000 ) ) ;
#6665 = MANIFOLD_SOLID_BREP ( 'Boss-Extrude1', #3227 ) ;
#6666 = ORIENTED_EDGE ( 'NONE', *, *, #3184, .T. ) ;
#6667 = ORIENTED_EDGE ( 'NONE', *, *, #2431, .T. ) ;
#6668 = CARTESIAN_POINT ( 'NONE',  ( 0.3442723180356911383, -0.3299850069800938646, -0.01900038327687023423 ) ) ;
#6669 = B_SPLINE_CURVE_WITH_KNOTS ( 'NONE', 3,
 ( #1002, #4452, #6702, #3293, #854, #1448 ),
 .UNSPECIFIED., .F., .F.,
 ( 4, 2, 4 ),
 ( 0.02625214965902978106, 0.02844383079405753134, 0.03063551192908527815 ),
 .UNSPECIFIED. ) ;
#6670 = CARTESIAN_POINT ( 'NONE',  ( 0.3543307086614173596, 0.000000000000000000, -0.4082677165354330340 ) ) ;
#6671 = ORIENTED_EDGE ( 'NONE', *, *, #3329, .F. ) ;
#6672 = CARTESIAN_POINT ( 'NONE',  ( 0.9697097892794954710, -0.4330708661417219663, -1.453662943332484803 ) ) ;
#6673 = ORIENTED_EDGE ( 'NONE', *, *, #5150, .T. ) ;
#6674 = CARTESIAN_POINT ( 'NONE',  ( -0.3543307086614173040, -0.06891495372886453918, -0.4052962681128434164 ) ) ;
#6675 = EDGE_LOOP ( 'NONE', ( #5556, #5529 ) ) ;
#6676 = B_SPLINE_CURVE_WITH_KNOTS ( 'NONE', 3,
 ( #3698, #5918, #4147, #2468, #1350, #4805 ),
 .UNSPECIFIED., .F., .F.,
 ( 4, 2, 4 ),
 ( 0.01452727543195640389, 0.01715716534226973539, 0.01978705525258306341 ),
 .UNSPECIFIED. ) ;
#6677 = CARTESIAN_POINT ( 'NONE',  ( 0.3581828924050323715, -0.1743168766271109560, 0.3019256869348722616 ) ) ;
#6678 = EDGE_CURVE ( 'NONE', #7079, #670, #5108, .T. ) ;
#6679 = DIRECTION ( 'NONE',  ( -0.000000000000000000, -0.000000000000000000, -1.000000000000000000 ) ) ;
#6680 = ORIENTED_EDGE ( 'NONE', *, *, #923, .F. ) ;
#6681 = CARTESIAN_POINT ( 'NONE',  ( 0.000000000000000000, 0.000000000000000000, 0.000000000000000000 ) ) ;
#6682 = CARTESIAN_POINT ( 'NONE',  ( 2.755905511811024056, 0.000000000000000000, -0.2362204724409449896 ) ) ;
#6683 = ADVANCED_FACE ( 'NONE', ( #5572 ), #6005, .T. ) ;
#6684 = ADVANCED_FACE ( 'NONE', ( #5612 ), #4644, .T. ) ;
#6685 = CARTESIAN_POINT ( 'NONE',  ( 0.4368170150760393167, 0.9411660957780392245, -1.456692913385826849 ) ) ;
#6686 = CARTESIAN_POINT ( 'NONE',  ( 0.3543307086614173040, 0.2045729300278199825, -0.4082677165354330340 ) ) ;
#6687 = ORIENTED_EDGE ( 'NONE', *, *, #459, .T. ) ;
#6688 = CONICAL_SURFACE ( 'NONE', #3017, 0.3543307086614173596, 1.047197551196596521 ) ;
#6689 = DIRECTION ( 'NONE',  ( -2.207829878515936732E-15, 0.000000000000000000, 1.000000000000000000 ) ) ;
#6690 = EDGE_CURVE ( 'NONE', #1074, #6852, #1341, .T. ) ;
#6691 = CARTESIAN_POINT ( 'NONE',  ( 0.2961551751698085488, -0.2381605899494511347, -0.3942397458900141483 ) ) ;
#6692 = CARTESIAN_POINT ( 'NONE',  ( 0.000000000000000000, 0.2559055118110236116, 0.000000000000000000 ) ) ;
#6693 = CARTESIAN_POINT ( 'NONE',  ( 0.000000000000000000, 0.000000000000000000, 0.000000000000000000 ) ) ;
#6694 = B_SPLINE_CURVE_WITH_KNOTS ( 'NONE', 3,
 ( #31, #6494, #682, #150, #6450, #1236 ),
 .UNSPECIFIED., .F., .F.,
 ( 4, 2, 4 ),
 ( 0.009270618776430218297, 0.01189894710419331023, 0.01452727543195640389 ),
 .UNSPECIFIED. ) ;
#6695 = AXIS2_PLACEMENT_3D ( 'NONE', #7515, #7109, #1868 ) ;
#6696 = EDGE_CURVE ( 'NONE', #6730, #5941, #6482, .T. ) ;
#6697 = CARTESIAN_POINT ( 'NONE',  ( -0.4353079511162236681, 0.9479499796399324385, -1.456692913385828625 ) ) ;
#6698 = VERTEX_POINT ( 'NONE', #899 ) ;
#6699 = FACE_OUTER_BOUND ( 'NONE', #901, .T. ) ;
#6700 = VECTOR ( 'NONE', #2535, 39.37007874015748143 ) ;
#6701 = ORIENTED_EDGE ( 'NONE', *, *, #382, .T. ) ;
#6702 = CARTESIAN_POINT ( 'NONE',  ( 0.002479217192763490639, -0.05744896992510376693, -0.2952755905511810774 ) ) ;
#6703 = CIRCLE ( 'NONE', #6335, 1.124634398195722973 ) ;
#6704 = CARTESIAN_POINT ( 'NONE',  ( -1.048552902599921843, 0.4330708661417285721, -1.573978973432616835 ) ) ;
#6705 = VERTEX_POINT ( 'NONE', #4991 ) ;
#6706 = CARTESIAN_POINT ( 'NONE',  ( 0.9783381746514295818, -0.4342019027940097198, -1.450123259817208909 ) ) ;
#6707 = ORIENTED_EDGE ( 'NONE', *, *, #5116, .F. ) ;
#6708 = CARTESIAN_POINT ( 'NONE',  ( 0.7796304418040825857, 0.1182802082656420201, 0.9771433015668254951 ) ) ;
#6709 = DIRECTION ( 'NONE',  ( 0.000000000000000000, 1.000000000000000000, 0.000000000000000000 ) ) ;
#6710 = ORIENTED_EDGE ( 'NONE', *, *, #2521, .F. ) ;
#6711 = CIRCLE ( 'NONE', #5626, 0.4507874015748032370 ) ;
#6712 = ORIENTED_EDGE ( 'NONE', *, *, #2292, .T. ) ;
#6713 = LINE ( 'NONE', #372, #5862 ) ;
#6714 = CARTESIAN_POINT ( 'NONE',  ( 0.9454567723360981502, -0.2331403729576253803, -0.9562426076827387211 ) ) ;
#6715 = AXIS2_PLACEMENT_3D ( 'NONE', #2635, #7359, #3532 ) ;
#6716 = CARTESIAN_POINT ( 'NONE',  ( 0.4630669964643910341, -1.085749034322389672, -1.535808346805854541 ) ) ;
#6717=STYLED_ITEM('',(#7587),#3913);
#6718 = CARTESIAN_POINT ( 'NONE',  ( 0.3336175750056032396, -0.05682581389661664484, 0.2952755905511811330 ) ) ;
#6719 = DIRECTION ( 'NONE',  ( 0.000000000000000000, 0.000000000000000000, -1.000000000000000000 ) ) ;
#6720 = DIRECTION ( 'NONE',  ( -1.000000000000000000, -0.000000000000000000, -0.000000000000000000 ) ) ;
#6721 = CARTESIAN_POINT ( 'NONE',  ( 0.9857970000181629500, -0.4541662050560733577, -1.560880783937514504 ) ) ;
#6722 = CARTESIAN_POINT ( 'NONE',  ( 0.9705345056685881211, 0.4659838021921174356, -1.550372027848885281 ) ) ;
#6723 = EDGE_LOOP ( 'NONE', ( #1707, #2088, #3697, #1642 ) ) ;
#6724 = CARTESIAN_POINT ( 'NONE',  ( 0.9055118110236223261, 0.7480314960629921295, -0.7480314960629921295 ) ) ;
#6725 = EDGE_CURVE ( 'NONE', #1261, #4818, #1594, .T. ) ;
#6726 = DIRECTION ( 'NONE',  ( 0.000000000000000000, 0.000000000000000000, 1.000000000000000000 ) ) ;
#6727 = CIRCLE ( 'NONE', #2694, 0.3543307086614173596 ) ;
#6728 = SHAPE_DEFINITION_REPRESENTATION ( #3195, #1307 ) ;
#6729 = CARTESIAN_POINT ( 'NONE',  ( 0.4339190921229451048, 0.9541934910893031807, -1.456692913385826849 ) ) ;
#6730 = VERTEX_POINT ( 'NONE', #4086 ) ;
#6731 = CARTESIAN_POINT ( 'NONE',  ( 0.3527008206095850196, -0.1709223649093223885, 0.2960462201727743770 ) ) ;
#6732 = EDGE_CURVE ( 'NONE', #3999, #5611, #2573, .T. ) ;
#6733 = EDGE_CURVE ( 'NONE', #7028, #2144, #2699, .T. ) ;
#6734 = ORIENTED_EDGE ( 'NONE', *, *, #3118, .F. ) ;
#6735 = PRODUCT_DEFINITION_SHAPE ( 'NONE', 'NONE',  #7529 ) ;
#6736 = ORIENTED_EDGE ( 'NONE', *, *, #1536, .T. ) ;
#6737 = FACE_OUTER_BOUND ( 'NONE', #6953, .T. ) ;
#6738 = SURFACE_SIDE_STYLE ('',( #362 ) ) ;
#6739 = ORIENTED_EDGE ( 'NONE', *, *, #7514, .F. ) ;
#6740 = CARTESIAN_POINT ( 'NONE',  ( 0.9941396836775518997, -0.4762527114669922734, -1.397361282224856671 ) ) ;
#6741 = EDGE_LOOP ( 'NONE', ( #5086, #1174, #5399, #7298 ) ) ;
#6742 = VECTOR ( 'NONE', #444, 39.37007874015748143 ) ;
#6743 = CARTESIAN_POINT ( 'NONE',  ( 0.3336175750056032951, -0.05682581389661717219, -0.2952755905511811330 ) ) ;
#6744 = ORIENTED_EDGE ( 'NONE', *, *, #2208, .T. ) ;
#6745 = CARTESIAN_POINT ( 'NONE',  ( 0.3459463601587901560, 0.1956820507697113742, 0.2516199270399913090 ) ) ;
#6746 = ORIENTED_EDGE ( 'NONE', *, *, #3262, .T. ) ;
#6747 = VECTOR ( 'NONE', #3225, 39.37007874015748143 ) ;
#6748 = ORIENTED_EDGE ( 'NONE', *, *, #6957, .T. ) ;
#6749 = DIRECTION ( 'NONE',  ( -0.04025208698423509562, -0.9991895563372418243, 6.938519009613952148E-16 ) ) ;
#6750 = CARTESIAN_POINT ( 'NONE',  ( 0.3561390657006783811, -0.1723301304999994843, -0.2984845417009731050 ) ) ;
#6751 = DIRECTION ( 'NONE',  ( -0.000000000000000000, 0.000000000000000000, -1.000000000000000000 ) ) ;
#6752 = CARTESIAN_POINT ( 'NONE',  ( 1.196402575039207328, -0.1050201062211118808, -0.9787371541722721391 ) ) ;
#6753 = AXIS2_PLACEMENT_3D ( 'NONE', #6542, #2399, #5350 ) ;
#6754 = AXIS2_PLACEMENT_3D ( 'NONE', #419, #4316, #4469 ) ;
#6755 = DIRECTION ( 'NONE',  ( -1.000000000000000000, 0.000000000000000000, 0.000000000000000000 ) ) ;
#6756 = CARTESIAN_POINT ( 'NONE',  ( 0.9228159122846772977, 0.2286155672763659219, -0.9573382785580841770 ) ) ;
#6757 = B_SPLINE_CURVE_WITH_KNOTS ( 'NONE', 3,
 ( #3921, #6392, #5692, #1137, #449, #4567, #2731, #5186 ),
 .UNSPECIFIED., .F., .F.,
 ( 4, 2, 2, 4 ),
 ( 0.005257893453559908843, 0.006567392922673239916, 0.007876892391786570122, 0.01049589133001323227 ),
 .UNSPECIFIED. ) ;
#6758 = AXIS2_PLACEMENT_3D ( 'NONE', #945, #1052, #5118 ) ;
#6759 = CARTESIAN_POINT ( 'NONE',  ( 0.3391892065151627111, 0.1988903486381581598, -0.2460629921259842312 ) ) ;
#6760 = FACE_BOUND ( 'NONE', #1253, .T. ) ;
#6761 = CARTESIAN_POINT ( 'NONE',  ( 1.968503937007874072, 1.496062992125984259, 0.2362204724409449619 ) ) ;
#6762 = CARTESIAN_POINT ( 'NONE',  ( 0.01165389088405563781, -0.1143408654217081682, 0.2952755905511811885 ) ) ;
#6763 = B_SPLINE_CURVE_WITH_KNOTS ( 'NONE', 3,
 ( #6677, #136, #3769, #4801, #6105, #3071, #6032, #1850, #6638, #181 ),
 .UNSPECIFIED., .F., .F.,
 ( 4, 2, 2, 2, 4 ),
 ( 0.000000000000000000, 0.002239656411828512290, 0.004479312823657024580, 0.006718969235485537303, 0.008958625647314049159 ),
 .UNSPECIFIED. ) ;
#6764 = ORIENTED_EDGE ( 'NONE', *, *, #6403, .T. ) ;
#6765 = CARTESIAN_POINT ( 'NONE',  ( 0.4685039370078740717, 0.000000000000000000, 0.000000000000000000 ) ) ;
#6766 = CARTESIAN_POINT ( 'NONE',  ( -0.4330708661417317362, -1.048552902599920955, -1.573978973432617279 ) ) ;
#6767 = APPLICATION_PROTOCOL_DEFINITION ( 'draft international standard', 'automotive_design', 1998, #4039 ) ;
#6768 = AXIS2_PLACEMENT_3D ( 'NONE', #6271, #3397, #4550 ) ;
#6769 = COLOUR_RGB ( '',0.7921568627450980005, 0.8196078431372548767, 0.9333333333333333481 ) ;
#6770 = PRODUCT_RELATED_PRODUCT_CATEGORY ( 'part', '', ( #6010 ) ) ;
#6771 = CARTESIAN_POINT ( 'NONE',  ( -0.9666437042230129340, -0.4330708661417356220, -1.454455828411337359 ) ) ;
#6772 = ORIENTED_EDGE ( 'NONE', *, *, #3329, .T. ) ;
#6773 = CARTESIAN_POINT ( 'NONE',  ( 1.075170037517937605, -0.4403525121893617778, -1.561970602951606946 ) ) ;
#6774 = DIRECTION ( 'NONE',  ( -0.000000000000000000, -0.000000000000000000, -1.000000000000000000 ) ) ;
#6775 = B_SPLINE_CURVE_WITH_KNOTS ( 'NONE', 3,
 ( #4350, #7282, #2061, #4582, #5260, #5836 ),
 .UNSPECIFIED., .F., .F.,
 ( 4, 2, 4 ),
 ( -3.269571951031369869E-06, 0.0001651384380483837840, 0.0003335464480477989433 ),
 .UNSPECIFIED. ) ;
#6776 = ORIENTED_EDGE ( 'NONE', *, *, #6090, .F. ) ;
#6777 = EDGE_LOOP ( 'NONE', ( #2188, #3130, #199, #819, #3067, #80 ) ) ;
#6778 = CARTESIAN_POINT ( 'NONE',  ( 1.068462032678259234E-16, -0.2629500981735136689, -0.1351082512106133171 ) ) ;
#6779 = CARTESIAN_POINT ( 'NONE',  ( 0.9960021845704828403, 0.4720891361949586806, -1.401719468380313360 ) ) ;
#6780 =( REPRESENTATION_RELATIONSHIP ('NONE','NONE', #303, #7075 ) REPRESENTATION_RELATIONSHIP_WITH_TRANSFORMATION ( #1637 )SHAPE_REPRESENTATION_RELATIONSHIP( ) );
#6781 = EDGE_CURVE ( 'NONE', #75, #3031, #5643, .T. ) ;
#6782 = DIRECTION ( 'NONE',  ( -0.000000000000000000, -0.000000000000000000, 1.000000000000000000 ) ) ;
#6783 = ORIENTED_EDGE ( 'NONE', *, *, #3656, .F. ) ;
#6784 = EDGE_CURVE ( 'NONE', #4696, #6209, #5944, .T. ) ;
#6785 = DIRECTION ( 'NONE',  ( -1.000000000000000000, -0.000000000000000000, -4.625929269271482167E-15 ) ) ;
#6786 = ORIENTED_EDGE ( 'NONE', *, *, #148, .F. ) ;
#6787 = CARTESIAN_POINT ( 'NONE',  ( 0.3581828924050324825, 0.3486337532542225226, 1.056976728655274672E-17 ) ) ;
#6788 = DIRECTION ( 'NONE',  ( -1.000000000000000000, 0.000000000000000000, 0.000000000000000000 ) ) ;
#6789 = ORIENTED_EDGE ( 'NONE', *, *, #1200, .F. ) ;
#6790 = ORIENTED_EDGE ( 'NONE', *, *, #3503, .F. ) ;
#6791 = DIRECTION ( 'NONE',  ( 0.8813569915457181159, 0.4724509005743147694, 3.878473467381653369E-16 ) ) ;
#6792 = B_SPLINE_CURVE_WITH_KNOTS ( 'NONE', 3,
 ( #1892, #5370, #5418, #133, #179, #4261, #5456, #1760, #4102, #2610, #4874, #6773, #4593, #5058, #1520, #5713, #2719, #2861 ),
 .UNSPECIFIED., .F., .F.,
 ( 4, 2, 2, 2, 2, 2, 2, 2, 4 ),
 ( -8.042425861386104689E-06, 0.0009212656149223902389, 0.001385919635314278395, 0.001850573655706166552, 0.002315227676098054709, 0.002779881696489942648, 0.003244535716881830588, 0.003476862727077775425, 0.003709189737273719829 ),
 .UNSPECIFIED. ) ;
#6793 = DIRECTION ( 'NONE',  ( 0.5000000000000006661, 0.8660254037844382635, -0.000000000000000000 ) ) ;
#6794 = EDGE_CURVE ( 'NONE', #997, #4290, #4157, .T. ) ;
#6795 = CARTESIAN_POINT ( 'NONE',  ( 0.8401230830384029957, -0.1877837920673497696, -0.9662117393330279524 ) ) ;
#6796 = CARTESIAN_POINT ( 'NONE',  ( 0.7480314960629922405, 1.220472440944881942, 2.480314960629921295 ) ) ;
#6797 =( NAMED_UNIT ( * ) SI_UNIT ( $, .STERADIAN. ) SOLID_ANGLE_UNIT ( ) );
#6798 = PRODUCT_DEFINITION_FORMATION_WITH_SPECIFIED_SOURCE ( 'ANY', '', #2452, .NOT_KNOWN. ) ;
#6799 = CARTESIAN_POINT ( 'NONE',  ( 0.3561390657006783811, 0.1723301304999986516, -0.2984845417009731605 ) ) ;
#6800 = DIRECTION ( 'NONE',  ( -1.000000000000000000, 0.000000000000000000, 0.000000000000000000 ) ) ;
#6801 = DIRECTION ( 'NONE',  ( -1.000000000000000000, 0.000000000000000000, 0.000000000000000000 ) ) ;
#6802 = DIRECTION ( 'NONE',  ( -0.7071067811865496822, 0.000000000000000000, 0.7071067811865453523 ) ) ;
#6803 = FACE_OUTER_BOUND ( 'NONE', #688, .T. ) ;
#6804 = CARTESIAN_POINT ( 'NONE',  ( -1.950024051643512521E-29, 1.861696953619914682E-15, -1.361499588670820771 ) ) ;
#6805 = ITEM_DEFINED_TRANSFORMATION ( 'NONE', 'NONE', #331,  #5166 ) ;
#6806 = CARTESIAN_POINT ( 'NONE',  ( 0.3391892065151630442, -0.3125419764313924764, -0.04921259842519686706 ) ) ;
#6807 = VERTEX_POINT ( 'NONE', #5313 ) ;
#6808 = CARTESIAN_POINT ( 'NONE',  ( 0.02637295201093723881, -0.1704774416898505729, -0.2952755905511810774 ) ) ;
#6809 = CARTESIAN_POINT ( 'NONE',  ( 0.3496875272944827695, 0.1667004943313749321, -0.3018174552735724547 ) ) ;
#6810 = EDGE_LOOP ( 'NONE', ( #6655, #2930, #775, #7128, #5088, #7076 ) ) ;
#6811 = CIRCLE ( 'NONE', #6570, 0.3543307086614172485 ) ;
#6812 = ORIENTED_EDGE ( 'NONE', *, *, #3703, .T. ) ;
#6813 = CARTESIAN_POINT ( 'NONE',  ( 0.000000000000000000, 0.000000000000000000, 0.000000000000000000 ) ) ;
#6814 = CARTESIAN_POINT ( 'NONE',  ( 0.9609181420092280934, 0.5141614760841562992, -1.361499588670821659 ) ) ;
#6815 = ORIENTED_EDGE ( 'NONE', *, *, #5281, .T. ) ;
#6816 = CYLINDRICAL_SURFACE ( 'NONE', #4506, 0.4921259842519685179 ) ;
#6817 = ORIENTED_EDGE ( 'NONE', *, *, #5672, .T. ) ;
#6818 = TOROIDAL_SURFACE ( 'NONE', #3891, 1.223643328182682621, 0.05905511811023622659 ) ;
#6819 = CARTESIAN_POINT ( 'NONE',  ( 0.000000000000000000, 0.000000000000000000, -1.515748031496062964 ) ) ;
#6820 = ORIENTED_EDGE ( 'NONE', *, *, #2161, .F. ) ;
#6821 = DIRECTION ( 'NONE',  ( -1.000000000000000000, -3.491481338843133355E-15, 0.000000000000000000 ) ) ;
#6822 = CARTESIAN_POINT ( 'NONE',  ( 0.4330708661417322913, -0.9604263920613176353, -1.456063616177414310 ) ) ;
#6823 = EDGE_LOOP ( 'NONE', ( #1447, #6174, #7116 ) ) ;
#6824 =( REPRESENTATION_RELATIONSHIP ('NONE','NONE', #303, #1307 ) REPRESENTATION_RELATIONSHIP_WITH_TRANSFORMATION ( #5202 )SHAPE_REPRESENTATION_RELATIONSHIP( ) );
#6825 = EDGE_CURVE ( 'NONE', #10, #1248, #5763, .T. ) ;
#6826 = VERTEX_POINT ( 'NONE', #2445 ) ;
#6827 = ADVANCED_FACE ( 'NONE', ( #7142, #3512, #4243 ), #4736, .F. ) ;
#6828 = CARTESIAN_POINT ( 'NONE',  ( 0.000000000000000000, 0.000000000000000000, -0.2362204724409449341 ) ) ;
#6829 = AXIS2_PLACEMENT_3D ( 'NONE', #6654, #7111, #1870 ) ;
#6830 = DIRECTION ( 'NONE',  ( -0.9081580167345473242, -0.4186275392765909653, 0.000000000000000000 ) ) ;
#6831 = LINE ( 'NONE', #2130, #5504 ) ;
#6832 = DIRECTION ( 'NONE',  ( -1.000000000000000000, 0.000000000000000000, 0.000000000000000000 ) ) ;
#6833 =( NAMED_UNIT ( * ) SI_UNIT ( $, .STERADIAN. ) SOLID_ANGLE_UNIT ( ) );
#6834 = AXIS2_PLACEMENT_3D ( 'NONE', #17, #6720, #1465 ) ;
#6835 = DIRECTION ( 'NONE',  ( -3.491481338843133750E-15, 1.000000000000000000, 4.625929269271482167E-15 ) ) ;
#6836 = EDGE_CURVE ( 'NONE', #951, #2228, #7, .T. ) ;
#6837 = EDGE_CURVE ( 'NONE', #6508, #4891, #7068, .T. ) ;
#6838 = CARTESIAN_POINT ( 'NONE',  ( 0.4338950423154144254, 1.037563309807724821, -1.574803149606299302 ) ) ;
#6839 = CARTESIAN_POINT ( 'NONE',  ( 2.892866454678787531E-17, 1.496062992125984259, 0.2362204724409449341 ) ) ;
#6840 = CARTESIAN_POINT ( 'NONE',  ( 0.3403864257300893703, -0.2263128404110642256, 0.1985658431051765538 ) ) ;
#6841 = CARTESIAN_POINT ( 'NONE',  ( 0.004822332172886149328, 0.2917300191221098293, 0.08525996588982816260 ) ) ;
#6842 = CIRCLE ( 'NONE', #7197, 0.2362204724409449064 ) ;
#6843 = ORIENTED_EDGE ( 'NONE', *, *, #2530, .F. ) ;
#6844 = DIRECTION ( 'NONE',  ( 0.000000000000000000, 0.000000000000000000, 1.000000000000000000 ) ) ;
#6845 = CONTEXT_DEPENDENT_SHAPE_REPRESENTATION ( #816, #7154 ) ;
#6846 = B_SPLINE_CURVE_WITH_KNOTS ( 'NONE', 3,
 ( #5562, #2564, #6731, #6095, #7335, #2639 ),
 .UNSPECIFIED., .F., .F.,
 ( 4, 2, 4 ),
 ( 0.000000000000000000, 0.0001677595217559109278, 0.0003355190435118218556 ),
 .UNSPECIFIED. ) ;
#6847 = EDGE_LOOP ( 'NONE', ( #5, #1344, #6239, #6616 ) ) ;
#6848 = CARTESIAN_POINT ( 'NONE',  ( 0.3565325103478086399, 0.3440765519545058160, 0.005406888575954027845 ) ) ;
#6849 = CARTESIAN_POINT ( 'NONE',  ( 0.3442723180357227797, 0.1814473180894613513, -0.2762752072743030474 ) ) ;
#6850 = VERTEX_POINT ( 'NONE', #653 ) ;
#6851=STYLED_ITEM('',(#7566),#6665);
#6852 = VERTEX_POINT ( 'NONE', #2927 ) ;
#6853 = DIRECTION ( 'NONE',  ( -0.000000000000000000, 1.000000000000000000, 0.000000000000000000 ) ) ;
#6854 = CARTESIAN_POINT ( 'NONE',  ( 0.3485777078273625817, 0.2029921329169074307, 0.2518088348849962799 ) ) ;
#6855 =( NAMED_UNIT ( * ) SI_UNIT ( $, .STERADIAN. ) SOLID_ANGLE_UNIT ( ) );
#6856 = VERTEX_POINT ( 'NONE', #6012 ) ;
#6857 = FACE_OUTER_BOUND ( 'NONE', #2539, .T. ) ;
#6858 = VERTEX_POINT ( 'NONE', #765 ) ;
#6859 = AXIS2_PLACEMENT_3D ( 'NONE', #3983, #3904, #6844 ) ;
#6860 = CARTESIAN_POINT ( 'NONE',  ( 0.000000000000000000, 0.000000000000000000, 0.1188976377952756375 ) ) ;
#6861 = SURFACE_STYLE_FILL_AREA ( #973 ) ;
#6862 = VERTEX_POINT ( 'NONE', #5237 ) ;
#6863 = CARTESIAN_POINT ( 'NONE',  ( 0.3410249605999788325, -0.02903799983316278366, -0.3014927230551917026 ) ) ;
#6864 = DIRECTION ( 'NONE',  ( 1.000000000000000222, 5.282475884117239969E-32, -5.734680261998398735E-18 ) ) ;
#6865 = TOROIDAL_SURFACE ( 'NONE', #4428, 1.223643328182681289, 0.05905511811023622659 ) ;
#6866 = CARTESIAN_POINT ( 'NONE',  ( -2.834645669291338432, 0.000000000000000000, 0.4724409448818898127 ) ) ;
#6867 = LINE ( 'NONE', #5117, #1223 ) ;
#6868 = ADVANCED_FACE ( 'NONE', ( #691 ), #2450, .T. ) ;
#6869 = AXIS2_PLACEMENT_3D ( 'NONE', #4646, #4109, #3500 ) ;
#6870 = DIRECTION ( 'NONE',  ( 0.000000000000000000, 1.000000000000000000, 0.000000000000000000 ) ) ;
#6871 = CARTESIAN_POINT ( 'NONE',  ( 0.9531588649300888338, 0.2346757028646479781, -0.9558707923556580832 ) ) ;
#6872 = B_SPLINE_CURVE_WITH_KNOTS ( 'NONE', 3,
 ( #7394, #4421, #6750, #1581, #2166, #1501 ),
 .UNSPECIFIED., .F., .F.,
 ( 4, 2, 4 ),
 ( -3.269571951031369869E-06, 0.0001651384380483837840, 0.0003335464480477989433 ),
 .UNSPECIFIED. ) ;
#6873 = ADVANCED_BREP_SHAPE_REPRESENTATION ( '', ( #4080, #5166 ), #4173 ) ;
#6874 = CIRCLE ( 'NONE', #4556, 1.089828288828796676 ) ;
#6875 = DIMENSIONAL_EXPONENTS ( 1.000000000000000000, 0.000000000000000000, 0.000000000000000000, 0.000000000000000000, 0.000000000000000000, 0.000000000000000000, 0.000000000000000000 ) ;
#6876 = DIRECTION ( 'NONE',  ( -0.000000000000000000, 1.000000000000000000, 1.224646799147353207E-16 ) ) ;
#6877 = LINE ( 'NONE', #1628, #7186 ) ;
#6878 = EDGE_CURVE ( 'NONE', #7079, #7275, #988, .T. ) ;
#6879 = DIRECTION ( 'NONE',  ( 0.000000000000000000, 0.000000000000000000, -1.000000000000000000 ) ) ;
#6880 = ADVANCED_FACE ( 'NONE', ( #3593 ), #5155, .T. ) ;
#6881 = ORIENTED_EDGE ( 'NONE', *, *, #3657, .T. ) ;
#6882 = DIRECTION ( 'NONE',  ( 0.000000000000000000, 0.000000000000000000, 1.000000000000000000 ) ) ;
#6883 = AXIS2_PLACEMENT_3D ( 'NONE', #1091, #1595, #2783 ) ;
#6884 = ORIENTED_EDGE ( 'NONE', *, *, #376, .T. ) ;
#6885 = CARTESIAN_POINT ( 'NONE',  ( 3.198568410424924124, 2.407012729153881203, 2.952755905511811108 ) ) ;
#6886 = DIRECTION ( 'NONE',  ( -0.000000000000000000, -1.000000000000000000, -0.000000000000000000 ) ) ;
#6887 = ITEM_DEFINED_TRANSFORMATION ( 'NONE', 'NONE', #2328,  #5166 ) ;
#6888 = CARTESIAN_POINT ( 'NONE',  ( -0.9921522615226823216, -0.4406689276647633435, -1.439080857166196159 ) ) ;
#6889 = ORIENTED_EDGE ( 'NONE', *, *, #979, .F. ) ;
#6890 = DIRECTION ( 'NONE',  ( 7.708596820178695308E-30, -2.207829878515936732E-15, 1.000000000000000000 ) ) ;
#6891 = CARTESIAN_POINT ( 'NONE',  ( 0.3426144402834003788, -0.2318662757222078041, 0.2014770286013906619 ) ) ;
#6892 = VERTEX_POINT ( 'NONE', #7114 ) ;
#6893 = ORIENTED_EDGE ( 'NONE', *, *, #3645, .F. ) ;
#6894 = CONICAL_SURFACE ( 'NONE', #4576, 0.4629062255509093782, 1.221730476396037490 ) ;
#6895 = CARTESIAN_POINT ( 'NONE',  ( 0.9228159122846772977, -0.2286155672763659219, 0.9573382785580841770 ) ) ;
#6896 = CARTESIAN_POINT ( 'NONE',  ( 1.968503937007874072, 1.496062992125984259, 0.4921259842519685179 ) ) ;
#6897 = ORIENTED_EDGE ( 'NONE', *, *, #1588, .F. ) ;
#6898 = CARTESIAN_POINT ( 'NONE',  ( 0.000000000000000000, 0.000000000000000000, 0.000000000000000000 ) ) ;
#6899 = ORIENTED_EDGE ( 'NONE', *, *, #2155, .F. ) ;
#6900 = DIRECTION ( 'NONE',  ( -1.000000000000000000, -0.000000000000000000, 0.000000000000000000 ) ) ;
#6901 = ORIENTED_EDGE ( 'NONE', *, *, #5240, .F. ) ;
#6902 = PLANE ( 'NONE',  #5922 ) ;
#6903 = CARTESIAN_POINT ( 'NONE',  ( 33.78363125245376608, 38.11143353299878811, 54.13003647711801136 ) ) ;
#6904 = CARTESIAN_POINT ( 'NONE',  ( 0.000000000000000000, 0.000000000000000000, 0.000000000000000000 ) ) ;
#6905 = DIRECTION ( 'NONE',  ( 0.000000000000000000, 0.000000000000000000, -1.000000000000000000 ) ) ;
#6906 = CARTESIAN_POINT ( 'NONE',  ( 0.01834252172841640063, -0.1843865549457986697, 0.2711842997036482683 ) ) ;
#6907 = EDGE_CURVE ( 'NONE', #7025, #4703, #2923, .T. ) ;
#6908 = DIRECTION ( 'NONE',  ( -1.000000000000000000, 0.000000000000000000, 0.000000000000000000 ) ) ;
#6909 = DIRECTION ( 'NONE',  ( -0.000000000000000000, -0.000000000000000000, 1.000000000000000000 ) ) ;
#6910 = DIRECTION ( 'NONE',  ( -0.000000000000000000, 0.000000000000000000, -1.000000000000000000 ) ) ;
#6911 = CARTESIAN_POINT ( 'NONE',  ( 0.000000000000000000, 0.000000000000000000, -0.4082677165354330340 ) ) ;
#6912 = CARTESIAN_POINT ( 'NONE',  ( 0.4330708661417322913, -0.9666437042230126009, -1.454455828411335583 ) ) ;
#6913 = EDGE_CURVE ( 'NONE', #3650, #5491, #515, .T. ) ;
#6914 = EDGE_CURVE ( 'NONE', #2290, #5274, #7200, .T. ) ;
#6915 = CARTESIAN_POINT ( 'NONE',  ( 0.2073036836782039261, 0.2894590224800283051, -0.4075196867561207692 ) ) ;
#6916 = CONTEXT_DEPENDENT_SHAPE_REPRESENTATION ( #7302, #6129 ) ;
#6917 = EDGE_CURVE ( 'NONE', #3331, #1068, #621, .T. ) ;
#6918 = CARTESIAN_POINT ( 'NONE',  ( -0.4330708661417322913, -0.9666437042230143772, -1.454455828411337359 ) ) ;
#6919 = EDGE_LOOP ( 'NONE', ( #780, #2451, #1179, #3564 ) ) ;
#6921 = CARTESIAN_POINT ( 'NONE',  ( 0.3426144402833972147, 0.2318662757222082205, -0.2014770286013785050 ) ) ;
#6920 = DIMENSIONAL_EXPONENTS ( 1.000000000000000000, 0.000000000000000000, 0.000000000000000000, 0.000000000000000000, 0.000000000000000000, 0.000000000000000000, 0.000000000000000000 ) ;
#6922 = CARTESIAN_POINT ( 'NONE',  ( 0.3479980290963757827, -0.3208941761713900997, 0.04760384692073289098 ) ) ;
#6923 =( REPRESENTATION_RELATIONSHIP ('NONE','NONE', #303, #5265 ) REPRESENTATION_RELATIONSHIP_WITH_TRANSFORMATION ( #3085 )SHAPE_REPRESENTATION_RELATIONSHIP( ) );
#6924 = ORIENTED_EDGE ( 'NONE', *, *, #4447, .F. ) ;
#6925 = VERTEX_POINT ( 'NONE', #803 ) ;
#6926 = EDGE_CURVE ( 'NONE', #4931, #2266, #1173, .T. ) ;
#6927 = DIRECTION ( 'NONE',  ( 0.000000000000000000, 0.000000000000000000, -1.000000000000000000 ) ) ;
#6928 = EDGE_CURVE ( 'NONE', #2762, #4592, #478, .T. ) ;
#6929 = CARTESIAN_POINT ( 'NONE',  ( 0.01168997831664888090, -0.3129651733100090039, 0.04847959992982862204 ) ) ;
#6930 = PLANE ( 'NONE',  #4738 ) ;
#6931 = ORIENTED_EDGE ( 'NONE', *, *, #6733, .T. ) ;
#6932 = CARTESIAN_POINT ( 'NONE',  ( 1.189145543181157505, 0.1185714375127665254, 0.9771702786582192601 ) ) ;
#6933 = B_SPLINE_CURVE_WITH_KNOTS ( 'NONE', 3,
 ( #3767, #6104, #5571, #254, #859, #6787 ),
 .UNSPECIFIED., .F., .F.,
 ( 4, 2, 4 ),
 ( 0.000000000000000000, 0.0001677595217559108194, 0.0003355190435118216388 ),
 .UNSPECIFIED. ) ;
#6934 = VECTOR ( 'NONE', #1786, 39.37007874015748143 ) ;
#6935 = CARTESIAN_POINT ( 'NONE',  ( 0.3581828924050324825, 0.3486337532542225226, 1.056976728655274672E-17 ) ) ;
#6936 = ORIENTED_EDGE ( 'NONE', *, *, #3270, .T. ) ;
#6937 = CARTESIAN_POINT ( 'NONE',  ( -0.5118110236220474452, 1.220472440944881942, 2.952755905511811108 ) ) ;
#6938 = CARTESIAN_POINT ( 'NONE',  ( 33.89456220083551585, 40.86510553865259254, 54.38831948726720356 ) ) ;
#6939 = AXIS2_PLACEMENT_3D ( 'NONE', #7370, #1094, #3946 ) ;
#6940 = CARTESIAN_POINT ( 'NONE',  ( 0.3483227611829849413, -0.3409548833797009237, 0.000000000000000000 ) ) ;
#6941 = DIRECTION ( 'NONE',  ( 0.000000000000000000, 1.000000000000000000, 0.000000000000000000 ) ) ;
#6942 = AXIS2_PLACEMENT_3D ( 'NONE', #6324, #7421, #3548 ) ;
#6943 =( NAMED_UNIT ( * ) SI_UNIT ( $, .STERADIAN. ) SOLID_ANGLE_UNIT ( ) );
#6944 = CARTESIAN_POINT ( 'NONE',  ( -1.126887297386508504E-15, -0.4091458600556405756, -0.3766201741223081378 ) ) ;
#6945 = AXIS2_PLACEMENT_3D ( 'NONE', #3278, #5630, #3319 ) ;
#6946 = CARTESIAN_POINT ( 'NONE',  ( -0.2362204724409449341, 2.892866454678787531E-17, 0.000000000000000000 ) ) ;
#6947 = CARTESIAN_POINT ( 'NONE',  ( 0.4338950423154144254, -1.037563309807725043, -1.574803149606299302 ) ) ;
#6948 = FACE_OUTER_BOUND ( 'NONE', #5496, .T. ) ;
#6949 = CONICAL_SURFACE ( 'NONE', #601, 0.3543307086614173596, 1.047197551196596521 ) ;
#6950 = DIRECTION ( 'NONE',  ( 1.000000000000000000, 0.000000000000000000, 0.000000000000000000 ) ) ;
#6951 = CARTESIAN_POINT ( 'NONE',  ( 0.3410249605999032263, -0.02920150297965336608, 0.3014927230551895931 ) ) ;
#6952 = CARTESIAN_POINT ( 'NONE',  ( -0.4475999628372195338, -0.9971723906835435747, -1.429777239771659048 ) ) ;
#6953 = EDGE_LOOP ( 'NONE', ( #3014, #2459, #585, #1724, #5361 ) ) ;
#6954 = CARTESIAN_POINT ( 'NONE',  ( -0.2699662542182227343, 3.306133091061471023E-17, 0.3732633159281743551 ) ) ;
#6955 = CIRCLE ( 'NONE', #4522, 0.2952755905511810774 ) ;
#6956 = PLANE ( 'NONE',  #5175 ) ;
#6957 = EDGE_CURVE ( 'NONE', #3631, #4410, #3095, .T. ) ;
#6958 = EDGE_LOOP ( 'NONE', ( #1446, #4339, #3358, #2324 ) ) ;
#6959 = EDGE_LOOP ( 'NONE', ( #6280, #363, #6884 ) ) ;
#6960 = CARTESIAN_POINT ( 'NONE',  ( 0.000000000000000000, 0.000000000000000000, -0.3865922971001068409 ) ) ;
#6961 = PRESENTATION_LAYER_ASSIGNMENT (  '', '', ( #6717 ) ) ;
#6962 = CARTESIAN_POINT ( 'NONE',  ( 0.3528971332113847725, 0.3341112492250003507, -0.02492269209175868722 ) ) ;
#6963 = ORIENTED_EDGE ( 'NONE', *, *, #3941, .F. ) ;
#6964 = CARTESIAN_POINT ( 'NONE',  ( -0.5141614760841420884, 0.000000000000000000, -2.204724409448823419 ) ) ;
#6965 = EDGE_CURVE ( 'NONE', #4341, #408, #3200, .T. ) ;
#6966 = EDGE_CURVE ( 'NONE', #662, #1000, #6676, .T. ) ;
#6967 = VECTOR ( 'NONE', #3192, 39.37007874015748143 ) ;
#6968 = CARTESIAN_POINT ( 'NONE',  ( -0.7480314960629922405, 1.220472440944881942, 2.480314960629921295 ) ) ;
#6969 = ORIENTED_EDGE ( 'NONE', *, *, #2615, .F. ) ;
#6970 = ADVANCED_FACE ( 'NONE', ( #2958 ), #5262, .T. ) ;
#6971 = CARTESIAN_POINT ( 'NONE',  ( 2.834645669291338432, 0.000000000000000000, 0.4724409448818898127 ) ) ;
#6972 = CARTESIAN_POINT ( 'NONE',  ( 27.32692456122369151, 45.20863634146751764, 54.79420970546445346 ) ) ;
#6973 = CARTESIAN_POINT ( 'NONE',  ( 0.02637295201093703412, 0.1704774416898499345, 0.2952755905511810774 ) ) ;
#6974 = AXIS2_PLACEMENT_3D ( 'NONE', #151, #4813, #6411 ) ;
#6975 = DIRECTION ( 'NONE',  ( -1.000000000000000000, -0.000000000000000000, -0.000000000000000000 ) ) ;
#6976 = CARTESIAN_POINT ( 'NONE',  ( 0.3432736861146661322, 0.3267484299055462005, -0.02460629921259842659 ) ) ;
#6977 = CARTESIAN_POINT ( 'NONE',  ( -0.4330708661417315142, 1.044891351410290214, -1.574550377471545470 ) ) ;
#6978 = CIRCLE ( 'NONE', #3688, 0.2362204724409448231 ) ;
#6979 = AXIS2_PLACEMENT_3D ( 'NONE', #2995, #6941, #1697 ) ;
#6980 = CARTESIAN_POINT ( 'NONE',  ( 0.3581828924050327045, -0.3486337532542230222, -1.123169198254405176E-18 ) ) ;
#6981 = AXIS2_PLACEMENT_3D ( 'NONE', #903, #3658, #3233 ) ;
#6982 = FACE_OUTER_BOUND ( 'NONE', #2418, .T. ) ;
#6983 = DIRECTION ( 'NONE',  ( 1.000000000000000000, 0.000000000000000000, 0.000000000000000000 ) ) ;
#6984 = FACE_OUTER_BOUND ( 'NONE', #4343, .T. ) ;
#6985 = AXIS2_PLACEMENT_3D ( 'NONE', #5806, #4041, #1151 ) ;
#6986 = CARTESIAN_POINT ( 'NONE',  ( 0.000000000000000000, 0.000000000000000000, -0.7983802283864783744 ) ) ;
#6987 = CARTESIAN_POINT ( 'NONE',  ( 0.3432736861146659657, 0.1846838951640041582, 0.2706692913385826960 ) ) ;
#6988 = CARTESIAN_POINT ( 'NONE',  ( 0.3574299024618896592, -0.1732824651941382854, 0.3001340337771306044 ) ) ;
#6989 = ORIENTED_EDGE ( 'NONE', *, *, #5272, .T. ) ;
#6990 = CARTESIAN_POINT ( 'NONE',  ( 0.000000000000000000, 0.000000000000000000, 0.000000000000000000 ) ) ;
#6991 = DIRECTION ( 'NONE',  ( -0.000000000000000000, -0.000000000000000000, 1.000000000000000000 ) ) ;
#6992 = EDGE_LOOP ( 'NONE', ( #4448, #6518 ) ) ;
#6993 = ORIENTED_EDGE ( 'NONE', *, *, #851, .T. ) ;
#6994 = CARTESIAN_POINT ( 'NONE',  ( 1.045688647185073705, -0.2282227683634086846, 0.9574297281001666882 ) ) ;
#6995 = EDGE_CURVE ( 'NONE', #7262, #5789, #2830, .T. ) ;
#6996 = CARTESIAN_POINT ( 'NONE',  ( 0.000000000000000000, 0.000000000000000000, -1.546597720061111847 ) ) ;
#6997 = CARTESIAN_POINT ( 'NONE',  ( 0.3581828924050323715, 0.1743168766271107895, -0.3019256869348722061 ) ) ;
#6998 = EDGE_LOOP ( 'NONE', ( #4379, #2896, #3876, #5858 ) ) ;
#6999 = CARTESIAN_POINT ( 'NONE',  ( 0.4882980771758823058, 0.9867934559254213367, -1.385219299502220336 ) ) ;
#7000 = CARTESIAN_POINT ( 'NONE',  ( -0.9755734897585901511, 0.4619485889667589995, -1.553989674004691901 ) ) ;
#7001 = VERTEX_POINT ( 'NONE', #5299 ) ;
#7002 = CIRCLE ( 'NONE', #3102, 0.03543307086614165546 ) ;
#7003 = DIRECTION ( 'NONE',  ( 1.000000000000000000, 0.000000000000000000, 0.000000000000000000 ) ) ;
#7004 = CARTESIAN_POINT ( 'NONE',  ( 0.3387173876318818611, 0.02883917696872971906, 0.2952755905511811330 ) ) ;
#7005 = EDGE_CURVE ( 'NONE', #1762, #5183, #5525, .T. ) ;
#7006 = ADVANCED_FACE ( 'NONE', ( #676 ), #6300, .F. ) ;
#7007 = DIRECTION ( 'NONE',  ( 0.000000000000000000, 0.000000000000000000, 1.000000000000000000 ) ) ;
#7008 = CIRCLE ( 'NONE', #2254, 0.2362204724409449341 ) ;
#7009 = ORIENTED_EDGE ( 'NONE', *, *, #5230, .T. ) ;
#7010 = ADVANCED_FACE ( 'NONE', ( #7016, #1768, #4108 ), #6442, .F. ) ;
#7011 = CARTESIAN_POINT ( 'NONE',  ( -0.4388997119412543779, -0.9346848099469042825, -1.455943619906243436 ) ) ;
#7012 = FACE_BOUND ( 'NONE', #5024, .T. ) ;
#7013 = ORIENTED_EDGE ( 'NONE', *, *, #3, .T. ) ;
#7014 = EDGE_CURVE ( 'NONE', #135, #3031, #2287, .T. ) ;
#7015 = LENGTH_MEASURE_WITH_UNIT ( LENGTH_MEASURE( 0.02539999999999999897 ), #4074 );
#7016 = FACE_BOUND ( 'NONE', #3450, .T. ) ;
#7017 = LINE ( 'NONE', #3000, #1743 ) ;
#7018 = FACE_OUTER_BOUND ( 'NONE', #4907, .T. ) ;
#7019 = CARTESIAN_POINT ( 'NONE',  ( 0.3585569304025113535, 0.1763492631043844516, -0.3019338371022697864 ) ) ;
#7020 = CARTESIAN_POINT ( 'NONE',  ( -0.9609181420092336445, 0.5141614760841427545, -1.361499588670819216 ) ) ;
#7021 = CARTESIAN_POINT ( 'NONE',  ( 1.220472440944881942, 0.7480314960629921295, 0.000000000000000000 ) ) ;
#7022 = PLANE ( 'NONE',  #1844 ) ;
#7023 = DIRECTION ( 'NONE',  ( 0.000000000000000000, 0.8660254037844375974, -0.5000000000000018874 ) ) ;
#7024 = DIRECTION ( 'NONE',  ( 0.000000000000000000, 0.000000000000000000, 1.000000000000000000 ) ) ;
#7025 = VERTEX_POINT ( 'NONE', #4400 ) ;
#7026 = DIRECTION ( 'NONE',  ( -0.000000000000000000, -0.000000000000000000, 1.000000000000000000 ) ) ;
#7027 = CARTESIAN_POINT ( 'NONE',  ( 0.000000000000000000, 0.000000000000000000, -1.574803149606299302 ) ) ;
#7028 = VERTEX_POINT ( 'NONE', #7292 ) ;
#7029 = EDGE_LOOP ( 'NONE', ( #3015, #1415, #1615 ) ) ;
#7030 = DIRECTION ( 'NONE',  ( 1.000000000000000000, 0.000000000000000000, 0.000000000000000000 ) ) ;
#7031 = AXIS2_PLACEMENT_3D ( 'NONE', #7040, #626, #13 ) ;
#7032 = CARTESIAN_POINT ( 'NONE',  ( 0.3410076799406683845, 0.2467857494855107137, -0.1755389823809322958 ) ) ;
#7033 = ORIENTED_EDGE ( 'NONE', *, *, #2666, .F. ) ;
#7034 = FACE_OUTER_BOUND ( 'NONE', #5526, .T. ) ;
#7035 = DIRECTION ( 'NONE',  ( 0.000000000000000000, 0.000000000000000000, -1.000000000000000000 ) ) ;
#7036 = CARTESIAN_POINT ( 'NONE',  ( -0.9861598787149308265, 0.4544645342395042809, -1.560495034967182004 ) ) ;
#7037 = ORIENTED_EDGE ( 'NONE', *, *, #1018, .F. ) ;
#7038 = DIRECTION ( 'NONE',  ( -1.000000000000000000, 0.000000000000000000, 0.000000000000000000 ) ) ;
#7039 = CARTESIAN_POINT ( 'NONE',  ( 0.3496875412996344190, 0.1780314126850971457, 0.2952755905511810774 ) ) ;
#7040 = CARTESIAN_POINT ( 'NONE',  ( 25.13671773485889815, 34.81515369617523703, 52.58546567498294166 ) ) ;
#7041 = CARTESIAN_POINT ( 'NONE',  ( 0.9964144355006142595, 2.543737003400971975E-44, -1.433776001880364026 ) ) ;
#7042 = ORIENTED_EDGE ( 'NONE', *, *, #1290, .F. ) ;
#7043 = CARTESIAN_POINT ( 'NONE',  ( -2.834645669291338432, 0.000000000000000000, 0.000000000000000000 ) ) ;
#7044 = CIRCLE ( 'NONE', #5834, 0.2362204724409448231 ) ;
#7045 = ORIENTED_EDGE ( 'NONE', *, *, #6690, .F. ) ;
#7046 = CARTESIAN_POINT ( 'NONE',  ( 6.221505307624544299E-30, -1.781909941321919274E-15, -1.397637795275591843 ) ) ;
#7047 = CARTESIAN_POINT ( 'NONE',  ( -1.023372273685338785, -0.4368378848980560281, -1.573834172653142627 ) ) ;
#7048 = ADVANCED_FACE ( 'NONE', ( #3174 ), #350, .F. ) ;
#7049 = ORIENTED_EDGE ( 'NONE', *, *, #1596, .F. ) ;
#7050 = UNCERTAINTY_MEASURE_WITH_UNIT (LENGTH_MEASURE( 1.000000000000000082E-05 ), #6262, 'distance_accuracy_value', 'NONE');
#7051 = CIRCLE ( 'NONE', #4374, 0.2362204724409449896 ) ;
#7052 = CARTESIAN_POINT ( 'NONE',  ( -0.4559215864680341013, 0.8989373009621118849, -1.445239633971736604 ) ) ;
#7053 = CYLINDRICAL_SURFACE ( 'NONE', #5914, 0.2362204724409449341 ) ;
#7054 = DIRECTION ( 'NONE',  ( -1.000000000000000000, 0.000000000000000000, 0.000000000000000000 ) ) ;
#7055 = AXIS2_PLACEMENT_3D ( 'NONE', #4199, #153, #1278 ) ;
#7056 = CARTESIAN_POINT ( 'NONE',  ( 0.4685039370078740717, 0.000000000000000000, 0.4507874015748032370 ) ) ;
#7057 = ADVANCED_FACE ( 'NONE', ( #5519 ), #7180, .T. ) ;
#7058 = EDGE_CURVE ( 'NONE', #2045, #3366, #7459, .T. ) ;
#7059 = CARTESIAN_POINT ( 'NONE',  ( 2.755905511811024056, 0.000000000000000000, 0.000000000000000000 ) ) ;
#7060 = DIRECTION ( 'NONE',  ( 3.491481338843133750E-15, -1.000000000000000000, -4.625929269271482167E-15 ) ) ;
#7061 = CARTESIAN_POINT ( 'NONE',  ( 0.3432736861146661322, 0.3267484299055463115, 0.02460629921259843353 ) ) ;
#7062 = VECTOR ( 'NONE', #7087, 39.37007874015748143 ) ;
#7063 = CARTESIAN_POINT ( 'NONE',  ( -5.385555596699467400E-15, 0.5141614760841421994, -2.204724409448823419 ) ) ;
#7064 = CARTESIAN_POINT ( 'NONE',  ( 0.3581828924050323715, 0.1743168766271109560, 0.3019256869348722616 ) ) ;
#7065 = FACE_BOUND ( 'NONE', #5458, .T. ) ;
#7066 = ORIENTED_EDGE ( 'NONE', *, *, #7509, .T. ) ;
#7067 = CARTESIAN_POINT ( 'NONE',  ( 0.3426147637089220765, 0.05832033309504411345, -0.3015404986019938893 ) ) ;
#7068 = LINE ( 'NONE', #1829, #4281 ) ;
#7069 = CIRCLE ( 'NONE', #4142, 0.3543307086614173596 ) ;
#7070 = VERTEX_POINT ( 'NONE', #3210 ) ;
#7071 = ORIENTED_EDGE ( 'NONE', *, *, #5676, .T. ) ;
#7072 = FACE_OUTER_BOUND ( 'NONE', #7442, .T. ) ;
#7073 = VECTOR ( 'NONE', #4957, 39.37007874015748143 ) ;
#7074 = DIRECTION ( 'NONE',  ( 0.000000000000000000, 0.000000000000000000, 1.000000000000000000 ) ) ;
#7075 = SHAPE_REPRESENTATION ( 'hex flange bolt small_iso_ISO 4162 - M12 x 30 x 30-N', ( #5166 ), #1473 ) ;
#7076 = ORIENTED_EDGE ( 'NONE', *, *, #4581, .T. ) ;
#7077 = CARTESIAN_POINT ( 'NONE',  ( 0.4406690496059742501, 0.9921524035015029108, -1.439080679658372608 ) ) ;
#7078 = DIRECTION ( 'NONE',  ( -1.000000000000000000, -0.000000000000000000, -0.000000000000000000 ) ) ;
#7079 = VERTEX_POINT ( 'NONE', #4328 ) ;
#7080 = DIRECTION ( 'NONE',  ( 1.000000000000000000, 0.000000000000000000, 0.000000000000000000 ) ) ;
#7081 = CARTESIAN_POINT ( 'NONE',  ( 0.4353079511162236126, -0.9479499796399308842, -1.456692913385826849 ) ) ;
#7082 = DIRECTION ( 'NONE',  ( 1.000000000000000000, 0.000000000000000000, 0.000000000000000000 ) ) ;
#7083 = SURFACE_STYLE_FILL_AREA ( #4257 ) ;
#7084 = CARTESIAN_POINT ( 'NONE',  ( 0.3487098613656773316, 0.1177053732609037312, 0.3017042368166658051 ) ) ;
#7085 = ORIENTED_EDGE ( 'NONE', *, *, #7428, .F. ) ;
#7086 = CARTESIAN_POINT ( 'NONE',  ( -1.063161251382697792, -0.4348450093584693699, -1.569784523562343770 ) ) ;
#7087 = DIRECTION ( 'NONE',  ( -0.000000000000000000, -1.000000000000000000, -0.000000000000000000 ) ) ;
#7088 = DIRECTION ( 'NONE',  ( 1.000000000000000000, 0.000000000000000000, 0.000000000000000000 ) ) ;
#7089 = ORIENTED_EDGE ( 'NONE', *, *, #2275, .F. ) ;
#7090 = AXIS2_PLACEMENT_3D ( 'NONE', #5934, #3713, #3170 ) ;
#7091 = EDGE_CURVE ( 'NONE', #3441, #3901, #7396, .T. ) ;
#7092 = FACE_OUTER_BOUND ( 'NONE', #4935, .T. ) ;
#7093 = CARTESIAN_POINT ( 'NONE',  ( -1.084813395429189642, 0.4713813068963866870, -1.526966363676886873 ) ) ;
#7094 = VECTOR ( 'NONE', #832, 39.37007874015748143 ) ;
#7095 = CARTESIAN_POINT ( 'NONE',  ( 0.3322355029819564209, 0.06185644463604170890, -0.2952755905511810774 ) ) ;
#7096 = CARTESIAN_POINT ( 'NONE',  ( 1.279527559055118280, 1.968503937007874072, 0.000000000000000000 ) ) ;
#7097 = PRODUCT_DEFINITION_CONTEXT ( 'detailed design', #1435, 'design' ) ;
#7098 = CARTESIAN_POINT ( 'NONE',  ( 0.000000000000000000, 1.496062992125984259, 0.000000000000000000 ) ) ;
#7099 = CIRCLE ( 'NONE', #3811, 0.2362204724409455170 ) ;
#7100 = CARTESIAN_POINT ( 'NONE',  ( 0.4388997119412543779, -0.9346848099469029503, -1.455943619906241215 ) ) ;
#7101 = CARTESIAN_POINT ( 'NONE',  ( 0.3528971332113847725, -0.1886393090946611450, -0.2768874834731246404 ) ) ;
#7102 = AXIS2_PLACEMENT_3D ( 'NONE', #2773, #5113, #7355 ) ;
#7103 = EDGE_CURVE ( 'NONE', #6925, #6629, #748, .T. ) ;
#7104 = ITEM_DEFINED_TRANSFORMATION ( 'NONE', 'NONE', #1155,  #5166 ) ;
#7105 = ADVANCED_FACE ( 'NONE', ( #1405 ), #6622, .T. ) ;
#7106 = CARTESIAN_POINT ( 'NONE',  ( 1.083679028610375239, 0.4756000659978086298, -1.522578585053779410 ) ) ;
#7107 = AXIS2_PLACEMENT_3D ( 'NONE', #6971, #1082, #2804 ) ;
#7108 = FACE_OUTER_BOUND ( 'NONE', #5411, .T. ) ;
#7109 = DIRECTION ( 'NONE',  ( 0.000000000000000000, 0.000000000000000000, -1.000000000000000000 ) ) ;
#7110 = DIRECTION ( 'NONE',  ( -0.7071067811865523467, 0.000000000000000000, 0.7071067811865426878 ) ) ;
#7111 = DIRECTION ( 'NONE',  ( 0.000000000000000000, 0.000000000000000000, 1.000000000000000000 ) ) ;
#7112 = VERTEX_POINT ( 'NONE', #3753 ) ;
#7113 = CARTESIAN_POINT ( 'NONE',  ( 1.968503937007874072, 0.000000000000000000, 0.9842519685039370358 ) ) ;
#7114 = CARTESIAN_POINT ( 'NONE',  ( 0.9479499796399277756, 0.4353079511162336046, -1.456692913385828625 ) ) ;
#7115 = AXIS2_PLACEMENT_3D ( 'NONE', #4077, #1770, #2277 ) ;
#7116 = ORIENTED_EDGE ( 'NONE', *, *, #6645, .F. ) ;
#7117 = VECTOR ( 'NONE', #5311, 39.37007874015748143 ) ;
#7118 = CARTESIAN_POINT ( 'NONE',  ( -0.1771653543307089018, -0.3068593950417300986, -0.4082677165354330340 ) ) ;
#7119 = EDGE_LOOP ( 'NONE', ( #6439, #5513, #6924, #4802, #7224, #82 ) ) ;
#7120 = DIRECTION ( 'NONE',  ( 5.296894631669315808E-46, -1.000000000000000000, 2.207829878515936732E-15 ) ) ;
#7121 = ORIENTED_EDGE ( 'NONE', *, *, #148, .T. ) ;
#7122 = VECTOR ( 'NONE', #3039, 39.37007874015748143 ) ;
#7123 = EDGE_LOOP ( 'NONE', ( #7422, #273, #348 ) ) ;
#7124 = CONTEXT_DEPENDENT_SHAPE_REPRESENTATION ( #5356, #4228 ) ;
#7125 = CARTESIAN_POINT ( 'NONE',  ( 0.3426140154788509529, 0.05854580700589206294, 0.3015405874046677703 ) ) ;
#7126 = ORIENTED_EDGE ( 'NONE', *, *, #6184, .F. ) ;
#7127 = CARTESIAN_POINT ( 'NONE',  ( 1.220472440944881720, 1.984939871850715226E-17, -0.9842519685039370358 ) ) ;
#7128 = ORIENTED_EDGE ( 'NONE', *, *, #5197, .T. ) ;
#7129 = SHAPE_REPRESENTATION_RELATIONSHIP ( 'NONE' , 'NONE' ,  #5531, #6873 ) ;
#7130 = AXIS2_PLACEMENT_3D ( 'NONE', #7098, #64, #4810 ) ;
#7131 = CARTESIAN_POINT ( 'NONE',  ( 0.0006233585804810778822, -0.2702164766613439628, -0.1225225144826657953 ) ) ;
#7132 = CARTESIAN_POINT ( 'NONE',  ( 0.7495315129468413939, -0.03083906941738260785, -0.9838885550255186407 ) ) ;
#7133 = CARTESIAN_POINT ( 'NONE',  ( 0.3528822938286762523, 0.1453909600788098055, -0.3018098512751524187 ) ) ;
#7134 = ADVANCED_FACE ( 'NONE', ( #6091 ), #3552, .T. ) ;
#7135 = CARTESIAN_POINT ( 'NONE',  ( 0.02637295201093722841, 0.3409548833797004797, 3.882420715168025960E-18 ) ) ;
#7136 = DIRECTION ( 'NONE',  ( 0.000000000000000000, 0.000000000000000000, 1.000000000000000000 ) ) ;
#7137 = CARTESIAN_POINT ( 'NONE',  ( 0.3306743754077736130, -0.2557161625347756373, -0.1476377952755904555 ) ) ;
#7138 = DIRECTION ( 'NONE',  ( -0.000000000000000000, 0.000000000000000000, -1.000000000000000000 ) ) ;
#7139 = CARTESIAN_POINT ( 'NONE',  ( 6.901988839087968355E-18, 0.4091458600556405201, -0.4082677165354330340 ) ) ;
#7140 = EDGE_LOOP ( 'NONE', ( #3833, #120, #2734, #5833 ) ) ;
#7141 = CARTESIAN_POINT ( 'NONE',  ( -4.536176542591435797E-15, 0.4330708661417287941, -2.204724409448822975 ) ) ;
#7142 = FACE_OUTER_BOUND ( 'NONE', #3216, .T. ) ;
#7143 = ADVANCED_FACE ( 'NONE', ( #3134 ), #4726, .F. ) ;
#7144 = ADVANCED_FACE ( 'NONE', ( #5201, #3364 ), #5674, .F. ) ;
#7145 = ORIENTED_EDGE ( 'NONE', *, *, #2615, .T. ) ;
#7146 = DIRECTION ( 'NONE',  ( 0.000000000000000000, 0.000000000000000000, -1.000000000000000000 ) ) ;
#7147 = EDGE_CURVE ( 'NONE', #1388, #4696, #4938, .T. ) ;
#7148 = CARTESIAN_POINT ( 'NONE',  ( 0.4341579107162097384, 1.060348520640340686, -1.570964845243103758 ) ) ;
#7149 = ORIENTED_EDGE ( 'NONE', *, *, #6732, .F. ) ;
#7150 = DIRECTION ( 'NONE',  ( 0.000000000000000000, 0.000000000000000000, -1.000000000000000000 ) ) ;
#7151 = EDGE_CURVE ( 'NONE', #3247, #428, #7210, .T. ) ;
#7152 = EDGE_CURVE ( 'NONE', #5611, #929, #5683, .T. ) ;
#7153 = VERTEX_POINT ( 'NONE', #5172 ) ;
#7154 = PRODUCT_DEFINITION_SHAPE ( 'NONE', 'NONE',  #7542 ) ;
#7155 = ORIENTED_EDGE ( 'NONE', *, *, #6556, .T. ) ;
#7156 = CARTESIAN_POINT ( 'NONE',  ( 0.3496875272944831026, -0.3447318307381757041, 0.006541864722391225496 ) ) ;
#7157 = CARTESIAN_POINT ( 'NONE',  ( 1.015186846506429985, -0.2347025779575657722, 0.9558642380754210910 ) ) ;
#7158 = CONTEXT_DEPENDENT_SHAPE_REPRESENTATION ( #5899, #3126 ) ;
#7159 = CARTESIAN_POINT ( 'NONE',  ( 0.3321019207957557895, 0.02907045490630093265, 0.2952755905511811330 ) ) ;
#7160 = ORIENTED_EDGE ( 'NONE', *, *, #2072, .T. ) ;
#7161 = CARTESIAN_POINT ( 'NONE',  ( -1.075169953371341913, -0.4403524516314022974, -1.561970681382795823 ) ) ;
#7162 = CARTESIAN_POINT ( 'NONE',  ( 0.3496779274129791504, 0.1667266398149495066, 0.3017721699676332303 ) ) ;
#7163 =( REPRESENTATION_RELATIONSHIP ('NONE','NONE', #303, #1552 ) REPRESENTATION_RELATIONSHIP_WITH_TRANSFORMATION ( #3475 )SHAPE_REPRESENTATION_RELATIONSHIP( ) );
#7164 = EDGE_LOOP ( 'NONE', ( #4941, #236, #4060, #2755 ) ) ;
#7165 = CARTESIAN_POINT ( 'NONE',  ( 0.3398312250858251948, -0.3151631602416472555, -0.04467257488985885983 ) ) ;
#7166 = CARTESIAN_POINT ( 'NONE',  ( 0.7556465724085326130, -0.06151677279835152806, -0.9824476696380366469 ) ) ;
#7167 = CARTESIAN_POINT ( 'NONE',  ( 0.02898191724071414593, 0.3924131423350827874, -0.3862808132025621344 ) ) ;
#7168 = CARTESIAN_POINT ( 'NONE',  ( 0.4921259842519683514, 0.000000000000000000, -2.204724409448820754 ) ) ;
#7169 = CARTESIAN_POINT ( 'NONE',  ( 0.4685039370078740717, 0.000000000000000000, 0.000000000000000000 ) ) ;
#7170 = CARTESIAN_POINT ( 'NONE',  ( 1.060348520640336467, 0.4341579107162202300, -1.570964845243103314 ) ) ;
#7171 = AXIS2_PLACEMENT_3D ( 'NONE', #3720, #1406, #5597 ) ;
#7172 = CARTESIAN_POINT ( 'NONE',  ( 0.3528850351813196951, 0.1886720902358826890, -0.2768301761068310274 ) ) ;
#7173 = CARTESIAN_POINT ( 'NONE',  ( -1.866451592287363150E-29, 1.781909941321919274E-15, -1.397637795275591843 ) ) ;
#7174 = CARTESIAN_POINT ( 'NONE',  ( 0.7480314960629922405, 1.220472440944881942, 0.4724409448818898127 ) ) ;
#7175 = CARTESIAN_POINT ( 'NONE',  ( -0.3543307086614173040, 0.2045729300278199547, -0.4082677165354330340 ) ) ;
#7176 = ORIENTED_EDGE ( 'NONE', *, *, #329, .T. ) ;
#7177 = CARTESIAN_POINT ( 'NONE',  ( 0.000000000000000000, 0.000000000000000000, 0.000000000000000000 ) ) ;
#7178 = CARTESIAN_POINT ( 'NONE',  ( -0.4330708661417317362, 1.048552902599920733, -1.573978973432617279 ) ) ;
#7179 = AXIS2_PLACEMENT_3D ( 'NONE', #1073, #3417, #648 ) ;
#7180 = CYLINDRICAL_SURFACE ( 'NONE', #4417, 0.7480314960629921295 ) ;
#7181 = B_SPLINE_CURVE_WITH_KNOTS ( 'NONE', 3,
 ( #5557, #804, #2108, #384, #4936, #4439 ),
 .UNSPECIFIED., .F., .F.,
 ( 4, 2, 4 ),
 ( 2.380732026380572752E-07, 0.002190927868076664002, 0.004381617662950689981 ),
 .UNSPECIFIED. ) ;
#7182 = CARTESIAN_POINT ( 'NONE',  ( -9.561467977824920278E-16, -0.4091458600556405756, -0.03164754241312491001 ) ) ;
#7183 = EDGE_CURVE ( 'NONE', #4943, #4985, #2818, .T. ) ;
#7184 = CARTESIAN_POINT ( 'NONE',  ( 0.01168997831664882192, -0.1984671517595423818, -0.2467959906213527677 ) ) ;
#7185 = ORIENTED_EDGE ( 'NONE', *, *, #1961, .F. ) ;
#7186 = VECTOR ( 'NONE', #5739, 39.37007874015748143 ) ;
#7187 = ORIENTED_EDGE ( 'NONE', *, *, #5808, .F. ) ;
#7188 = VERTEX_POINT ( 'NONE', #2179 ) ;
#7189 = CARTESIAN_POINT ( 'NONE',  ( 0.3565422270302660013, -0.3441025489056189213, 0.005451916616122784963 ) ) ;
#7190 = AXIS2_PLACEMENT_3D ( 'NONE', #7454, #6205, #1489 ) ;
#7191 = EDGE_CURVE ( 'NONE', #5146, #383, #2465, .T. ) ;
#7192 = CARTESIAN_POINT ( 'NONE',  ( 0.01834252172841640063, -0.1843865549457986697, 0.2711842997036482683 ) ) ;
#7193 = ADVANCED_FACE ( 'NONE', ( #2257 ), #6341, .T. ) ;
#7194 = CARTESIAN_POINT ( 'NONE',  ( 0.3565422270302657237, 0.3441025489056184772, -0.005451916616122978385 ) ) ;
#7195 = ORIENTED_EDGE ( 'NONE', *, *, #4259, .F. ) ;
#7196 = CARTESIAN_POINT ( 'NONE',  ( 0.7965271477292853453, 0.1442139612367993318, 0.9737154292565876057 ) ) ;
#7197 = AXIS2_PLACEMENT_3D ( 'NONE', #1458, #826, #3809 ) ;
#7198 = EDGE_CURVE ( 'NONE', #6087, #4293, #2220, .T. ) ;
#7199 = ORIENTED_EDGE ( 'NONE', *, *, #2928, .T. ) ;
#7200 = B_SPLINE_CURVE_WITH_KNOTS ( 'NONE', 3,
 ( #1367, #7217, #841, #7257, #4933, #2595, #876, #4324, #4852, #3749, #272, #6658, #6054, #4357, #1991, #5555, #1402, #7178 ),
 .UNSPECIFIED., .F., .F.,
 ( 4, 2, 2, 2, 2, 2, 2, 2, 4 ),
 ( -8.042425861385237327E-06, 0.0009212656149223862273, 0.001385919635314276878, 0.001850573655706167636, 0.002315227676098058178, 0.002779881696489948720, 0.003244535716881839262, 0.003476862727077780196, 0.003709189737273721130 ),
 .UNSPECIFIED. ) ;
#7201 = CARTESIAN_POINT ( 'NONE',  ( 0.000000000000000000, 0.000000000000000000, 0.3732633159281743551 ) ) ;
#7202 = CARTESIAN_POINT ( 'NONE',  ( -0.9842519685039370358, 1.220472440944881942, 2.480314960629921295 ) ) ;
#7203 = CARTESIAN_POINT ( 'NONE',  ( 0.8062609481994166272, -0.1560654929534785462, -0.9718629971449804783 ) ) ;
#7204 =( REPRESENTATION_RELATIONSHIP ('NONE','NONE', #303, #5531 ) REPRESENTATION_RELATIONSHIP_WITH_TRANSFORMATION ( #3829 )SHAPE_REPRESENTATION_RELATIONSHIP( ) );
#7205 = DIRECTION ( 'NONE',  ( 1.000000000000000000, 0.000000000000000000, 0.000000000000000000 ) ) ;
#7206 = AXIS2_PLACEMENT_3D ( 'NONE', #295, #2503, #2614 ) ;
#7207 = CARTESIAN_POINT ( 'NONE',  ( 0.3410249605999410294, -1.062517223525361548E-12, -0.3014927230551905368 ) ) ;
#7208 = FACE_OUTER_BOUND ( 'NONE', #5847, .T. ) ;
#7209 = CARTESIAN_POINT ( 'NONE',  ( 1.085572762089306531, 0.4589126309195485365, -1.540322683979783447 ) ) ;
#7210 = CIRCLE ( 'NONE', #4046, 0.2362204724409448231 ) ;
#7211 = CARTESIAN_POINT ( 'NONE',  ( 2.755905511811024056, 1.496062992125984259, 0.000000000000000000 ) ) ;
#7212 = CARTESIAN_POINT ( 'NONE',  ( 0.3426404862726870615, 0.2318193597401792261, 0.2015595396344879719 ) ) ;
#7213 = CYLINDRICAL_SURFACE ( 'NONE', #2062, 0.2362204724409449896 ) ;
#7214 = EDGE_LOOP ( 'NONE', ( #1432, #4835, #7121, #4262, #7049, #5722 ) ) ;
#7215 = PRODUCT_DEFINITION_SHAPE ( 'NONE', 'NONE',  #7549 ) ;
#7216 = CARTESIAN_POINT ( 'NONE',  ( 0.3391892065151631552, -0.3125419764313924209, 0.04921259842519686012 ) ) ;
#7217 = CARTESIAN_POINT ( 'NONE',  ( -0.5072158114897864500, 1.064252964791886580, -1.491281854711272059 ) ) ;
#7218 = ORIENTED_EDGE ( 'NONE', *, *, #7505, .F. ) ;
#7219 = AXIS2_PLACEMENT_3D ( 'NONE', #4995, #411, #6864 ) ;
#7220 = CARTESIAN_POINT ( 'NONE',  ( 0.3581828924050323715, 0.1743168766271107895, -0.3019256869348722061 ) ) ;
#7221 = CARTESIAN_POINT ( 'NONE',  ( 0.000000000000000000, 1.496062992125984259, 0.000000000000000000 ) ) ;
#7222 = VECTOR ( 'NONE', #3635, 39.37007874015748143 ) ;
#7223 = CARTESIAN_POINT ( 'NONE',  ( 0.4353079511162236126, 0.9479499796399308842, -1.456692913385826849 ) ) ;
#7224 = ORIENTED_EDGE ( 'NONE', *, *, #2116, .T. ) ;
#7225 = AXIS2_PLACEMENT_3D ( 'NONE', #3342, #2763, #5790 ) ;
#7226 = DIRECTION ( 'NONE',  ( 1.000000000000000000, 0.000000000000000000, 0.000000000000000000 ) ) ;
#7227 = B_SPLINE_CURVE_WITH_KNOTS ( 'NONE', 3,
 ( #4643, #1226, #6977, #5159 ),
 .UNSPECIFIED., .F., .F.,
 ( 4, 4 ),
 ( 6.648767611728002819E-17, 0.0002807012396508846487 ),
 .UNSPECIFIED. ) ;
#7228 = ORIENTED_EDGE ( 'NONE', *, *, #6126, .T. ) ;
#7229 = EDGE_CURVE ( 'NONE', #4054, #3405, #5400, .T. ) ;
#7230 = EDGE_LOOP ( 'NONE', ( #4403, #1994, #6584, #5062 ) ) ;
#7231 = CONICAL_SURFACE ( 'NONE', #640, 0.2952755905511810774, 1.047197551196600518 ) ;
#7232 = CARTESIAN_POINT ( 'NONE',  ( 2.755905511811024056, 1.496062992125984259, 0.000000000000000000 ) ) ;
#7233 = CARTESIAN_POINT ( 'NONE',  ( 0.1771653543307088463, -0.3068593950417300431, 7.886165872636028972E-17 ) ) ;
#7234 = CARTESIAN_POINT ( 'NONE',  ( 0.3398312250857989381, 0.3151631602416481437, 0.04467257488985636182 ) ) ;
#7235 = ORIENTED_EDGE ( 'NONE', *, *, #2941, .F. ) ;
#7236 = CARTESIAN_POINT ( 'NONE',  ( 0.7601650273709252836, 0.07630400123961592063, 0.9813937435533869325 ) ) ;
#7237 = VERTEX_POINT ( 'NONE', #1705 ) ;
#7238 = DIRECTION ( 'NONE',  ( 0.000000000000000000, 1.000000000000000000, 0.000000000000000000 ) ) ;
#7239 = CONICAL_SURFACE ( 'NONE', #2825, 0.3543307086614173596, 1.047197551196596521 ) ;
#7240 = DIRECTION ( 'NONE',  ( -1.000000000000000000, 0.000000000000000000, -0.000000000000000000 ) ) ;
#7241 = EDGE_CURVE ( 'NONE', #1329, #3366, #2931, .T. ) ;
#7242 = EDGE_LOOP ( 'NONE', ( #4902, #1710, #238 ) ) ;
#7243 = EDGE_CURVE ( 'NONE', #1005, #913, #14, .T. ) ;
#7244 = DIRECTION ( 'NONE',  ( 0.000000000000000000, 0.000000000000000000, 1.000000000000000000 ) ) ;
#7245 = EDGE_CURVE ( 'NONE', #7450, #7153, #7511, .T. ) ;
#7246 = FACE_OUTER_BOUND ( 'NONE', #486, .T. ) ;
#7247 = CARTESIAN_POINT ( 'NONE',  ( 1.171887040486664588, -0.1443386382778019672, -0.9736977440596933375 ) ) ;
#7248 =( GEOMETRIC_REPRESENTATION_CONTEXT ( 3 ) GLOBAL_UNCERTAINTY_ASSIGNED_CONTEXT ( ( #3359 ) ) GLOBAL_UNIT_ASSIGNED_CONTEXT ( ( #1271, #3579, #6443 ) ) REPRESENTATION_CONTEXT ( 'NONE', 'WORKASPACE' ) );
#7249 = CARTESIAN_POINT ( 'NONE',  ( 0.4878045971889972132, -1.078368813366570533, -1.510181706589752482 ) ) ;
#7250 = EDGE_CURVE ( 'NONE', #6209, #2382, #3471, .T. ) ;
#7251 = CARTESIAN_POINT ( 'NONE',  ( 0.3432736861146659657, -0.1420645347415416260, 0.2952755905511810774 ) ) ;
#7252 = CARTESIAN_POINT ( 'NONE',  ( 0.4700904924197906176, 0.8785537298370117432, -1.433776001880362250 ) ) ;
#7253 = CARTESIAN_POINT ( 'NONE',  ( -0.5118110236220474452, 1.220472440944881942, 0.4724409448818898127 ) ) ;
#7254 = ORIENTED_EDGE ( 'NONE', *, *, #1336, .F. ) ;
#7255 = AXIS2_PLACEMENT_3D ( 'NONE', #6429, #2944, #6470 ) ;
#7256 = DIRECTION ( 'NONE',  ( -1.000000000000000000, 0.000000000000000000, -2.256009703088257329E-15 ) ) ;
#7257 = CARTESIAN_POINT ( 'NONE',  ( -0.4878048847236817753, 1.078368654584403563, -1.510181419419387661 ) ) ;
#7258 = ORIENTED_EDGE ( 'NONE', *, *, #3280, .T. ) ;
#7259 = DIRECTION ( 'NONE',  ( -0.7071067811865523467, 8.659560562354873694E-17, -0.7071067811865426878 ) ) ;
#7260 = CARTESIAN_POINT ( 'NONE',  ( 0.000000000000000000, 0.000000000000000000, -0.2952755905511810774 ) ) ;
#7261 = CARTESIAN_POINT ( 'NONE',  ( 0.5141614760841458631, 1.056523642887403192, -1.484898342931014303 ) ) ;
#7262 = VERTEX_POINT ( 'NONE', #32 ) ;
#7263 = CARTESIAN_POINT ( 'NONE',  ( 2.834645669291338876, 0.4724409448818890911, 8.169257281319195485 ) ) ;
#7264 = ORIENTED_EDGE ( 'NONE', *, *, #1811, .F. ) ;
#7265 = ORIENTED_EDGE ( 'NONE', *, *, #5850, .T. ) ;
#7266 = CARTESIAN_POINT ( 'NONE',  ( 0.4685039370078740717, 0.1704774416898499345, 0.2952755905511810774 ) ) ;
#7267 = CYLINDRICAL_SURFACE ( 'NONE', #2778, 0.2362204724409446843 ) ;
#7268 = CARTESIAN_POINT ( 'NONE',  ( 0.9867934559254264437, -0.4882980771758718697, -1.385219299502220114 ) ) ;
#7269 = ORIENTED_EDGE ( 'NONE', *, *, #83, .F. ) ;
#7270 = CARTESIAN_POINT ( 'NONE',  ( 0.9479499796399352141, -0.4353079511162137316, -1.456692913385826849 ) ) ;
#7271 = PRODUCT_RELATED_PRODUCT_CATEGORY ( 'part', '', ( #4837 ) ) ;
#7272 = ORIENTED_EDGE ( 'NONE', *, *, #3088, .F. ) ;
#7273 = DIRECTION ( 'NONE',  ( 1.000000000000000000, 0.000000000000000000, 0.000000000000000000 ) ) ;
#7274 = ORIENTED_EDGE ( 'NONE', *, *, #4303, .T. ) ;
#7275 = VERTEX_POINT ( 'NONE', #2964 ) ;
#7276 = PRODUCT_DEFINITION_SHAPE ( 'NONE', 'NONE',  #7525 ) ;
#7277 = DIRECTION ( 'NONE',  ( -1.000000000000000000, 0.000000000000000000, 0.000000000000000000 ) ) ;
#7278 = CARTESIAN_POINT ( 'NONE',  ( 1.162034203329631143, -0.1562967039942805003, -0.9718251695195749829 ) ) ;
#7279 = EDGE_CURVE ( 'NONE', #75, #3292, #6212, .T. ) ;
#7280 = CARTESIAN_POINT ( 'NONE',  ( -0.8884022185686297757, -0.4627504720074800404, -1.439912370850676027 ) ) ;
#7281 = CARTESIAN_POINT ( 'NONE',  ( -0.9666437042230142662, 0.4330708661417289052, -1.454455828411335583 ) ) ;
#7282 = CARTESIAN_POINT ( 'NONE',  ( 0.3574269917172684941, -0.1732784665916271005, -0.3001271079943088615 ) ) ;
#7283 = EDGE_CURVE ( 'NONE', #1378, #6705, #5881, .T. ) ;
#7284 = CARTESIAN_POINT ( 'NONE',  ( 1.044891351410292435, -0.4330708661417213556, -1.574550377471545692 ) ) ;
#7285 = EDGE_CURVE ( 'NONE', #5278, #709, #2323, .T. ) ;
#7286 = VERTEX_POINT ( 'NONE', #4650 ) ;
#7287 = COLOUR_RGB ( '',0.7921568627450980005, 0.8196078431372548767, 0.9333333333333333481 ) ;
#7288 = LINE ( 'NONE', #6724, #1011 ) ;
#7289 = B_SPLINE_CURVE_WITH_KNOTS ( 'NONE', 3,
 ( #994, #3211, #7512, #5812, #1635, #3399 ),
 .UNSPECIFIED., .F., .F.,
 ( 4, 2, 4 ),
 ( 2.380732026382070147E-07, 0.002190927868076674410, 0.004381617662950710798 ),
 .UNSPECIFIED. ) ;
#7290 = EDGE_LOOP ( 'NONE', ( #6199, #4087, #2040, #6899 ) ) ;
#7291 = CARTESIAN_POINT ( 'NONE',  ( -0.1771653543307089573, 0.3068593950417301541, 0.000000000000000000 ) ) ;
#7292 = CARTESIAN_POINT ( 'NONE',  ( -1.089828288828796898, 1.213184216936748681E-31, -1.361499588670820771 ) ) ;
#7293 = DIRECTION ( 'NONE',  ( 0.3420201433256623291, 0.000000000000000000, -0.9396926207859106484 ) ) ;
#7294 = AXIS2_PLACEMENT_3D ( 'NONE', #919, #2562, #241 ) ;
#7295 = CARTESIAN_POINT ( 'NONE',  ( 0.4713815370807412641, 1.084813347358863478, -1.526966122205014820 ) ) ;
#7296 = VERTEX_POINT ( 'NONE', #6495 ) ;
#7297 = DIRECTION ( 'NONE',  ( -1.000000000000000000, -0.000000000000000000, 0.000000000000000000 ) ) ;
#7298 = ORIENTED_EDGE ( 'NONE', *, *, #6836, .F. ) ;
#7299 = ORIENTED_EDGE ( 'NONE', *, *, #5844, .T. ) ;
#7300 = DIRECTION ( 'NONE',  ( 1.000000000000000000, 0.000000000000000000, -0.000000000000000000 ) ) ;
#7301 = CARTESIAN_POINT ( 'NONE',  ( 0.9941396836775437951, 0.4762527114670134232, -1.397361282224859780 ) ) ;
#7302 =( REPRESENTATION_RELATIONSHIP ('NONE','NONE', #303, #1552 ) REPRESENTATION_RELATIONSHIP_WITH_TRANSFORMATION ( #7483 )SHAPE_REPRESENTATION_RELATIONSHIP( ) );
#7303 = AXIS2_PLACEMENT_3D ( 'NONE', #7063, #4814, #5041 ) ;
#7304 = CARTESIAN_POINT ( 'NONE',  ( 7.874015748031496287, 0.2559055118110236116, -0.4921259842519685179 ) ) ;
#7305 = B_SPLINE_CURVE_WITH_KNOTS ( 'NONE', 3,
 ( #2244, #557, #1660, #1583 ),
 .UNSPECIFIED., .F., .F.,
 ( 4, 4 ),
 ( 0.000000000000000000, 0.0004815725036528575279 ),
 .UNSPECIFIED. ) ;
#7306 = CARTESIAN_POINT ( 'NONE',  ( -0.1171731013849884873, -0.3414959384292345357, -0.003016182236739476611 ) ) ;
#7307 = ORIENTED_EDGE ( 'NONE', *, *, #1343, .F. ) ;
#7308 = CARTESIAN_POINT ( 'NONE',  ( 0.9685300475558180633, 0.2358242948353262147, 0.9555833128140062138 ) ) ;
#7309 = ORIENTED_EDGE ( 'NONE', *, *, #2879, .F. ) ;
#7310 = LENGTH_MEASURE_WITH_UNIT ( LENGTH_MEASURE( 0.02539999999999999897 ), #4414 );
#7311 = ORIENTED_EDGE ( 'NONE', *, *, #1639, .F. ) ;
#7312 = AXIS2_PLACEMENT_3D ( 'NONE', #3062, #5324, #4795 ) ;
#7313 = DIRECTION ( 'NONE',  ( -1.000000000000000000, -8.648785545355717899E-18, -2.320548612096681119E-16 ) ) ;
#7314 = CARTESIAN_POINT ( 'NONE',  ( 0.000000000000000000, -0.2557161625347748601, 0.1476377952755911216 ) ) ;
#7315 =( CONVERSION_BASED_UNIT ( 'INCH', #2654 ) LENGTH_UNIT ( ) NAMED_UNIT ( #5759 ) );
#7316 = AXIS2_PLACEMENT_3D ( 'NONE', #495, #5221, #6832 ) ;
#7317 = CARTESIAN_POINT ( 'NONE',  ( 7.874015748031496287, 0.2559055118110236116, 0.000000000000000000 ) ) ;
#7318 = B_SPLINE_CURVE_WITH_KNOTS ( 'NONE', 3,
 ( #5919, #6485, #4191, #3578 ),
 .UNSPECIFIED., .F., .F.,
 ( 4, 4 ),
 ( 6.648767611728001586E-17, 0.0002807012396508843776 ),
 .UNSPECIFIED. ) ;
#7319 = CIRCLE ( 'NONE', #2087, 0.2948818897637794922 ) ;
#7320 = EDGE_CURVE ( 'NONE', #1804, #6698, #6371, .T. ) ;
#7321 = DIRECTION ( 'NONE',  ( 0.000000000000000000, 0.000000000000000000, -1.000000000000000000 ) ) ;
#7322 = CARTESIAN_POINT ( 'NONE',  ( 0.000000000000000000, 0.000000000000000000, -0.2362204724409449341 ) ) ;
#7323 = CARTESIAN_POINT ( 'NONE',  ( 0.0006233585804808155053, 0.2702164766613434077, 0.1225225144826656842 ) ) ;
#7324 = CARTESIAN_POINT ( 'NONE',  ( 1.010073413237861928, 0.4416276115803188240, -1.570717210673253428 ) ) ;
#7325 = VERTEX_POINT ( 'NONE', #2392 ) ;
#7326 = DIRECTION ( 'NONE',  ( 0.000000000000000000, -0.5000000000000012212, -0.8660254037844377084 ) ) ;
#7327 = ORIENTED_EDGE ( 'NONE', *, *, #4347, .T. ) ;
#7328 = CARTESIAN_POINT ( 'NONE',  ( 0.3483227611829846082, 0.1704774416898497680, -0.2952755905511810774 ) ) ;
#7329 = ADVANCED_FACE ( 'NONE', ( #3544 ), #66, .F. ) ;
#7330 = EDGE_CURVE ( 'NONE', #2214, #2732, #1600, .T. ) ;
#7331 = DIRECTION ( 'NONE',  ( -1.224646799147353207E-16, 1.000000000000000000, 0.000000000000000000 ) ) ;
#7332 = EDGE_CURVE ( 'NONE', #1484, #4949, #993, .T. ) ;
#7333 = CARTESIAN_POINT ( 'NONE',  ( 0.2962704110120346068, 0.2380940585049209079, -0.01405589313879318687 ) ) ;
#7334 = ORIENTED_EDGE ( 'NONE', *, *, #2712, .F. ) ;
#7335 = CARTESIAN_POINT ( 'NONE',  ( 0.3574299024618896592, -0.1732824651941382854, 0.3001340337771306044 ) ) ;
#7336 = AXIS2_PLACEMENT_3D ( 'NONE', #6693, #3863, #1440 ) ;
#7337 = ORIENTED_EDGE ( 'NONE', *, *, #6639, .F. ) ;
#7338 = AXIS2_PLACEMENT_3D ( 'NONE', #5976, #167, #7146 ) ;
#7339 = ORIENTED_EDGE ( 'NONE', *, *, #6543, .T. ) ;
#7340 = EDGE_CURVE ( 'NONE', #5905, #2762, #115, .T. ) ;
#7341 = CARTESIAN_POINT ( 'NONE',  ( 0.000000000000000000, -0.2557161625347750822, -0.1476377952755907330 ) ) ;
#7342 = CARTESIAN_POINT ( 'NONE',  ( 0.3426404862726870615, 0.2318193597401792261, 0.2015595396344879719 ) ) ;
#7343=STYLED_ITEM('',(#7587),#6540);
#7344 =( GEOMETRIC_REPRESENTATION_CONTEXT ( 3 ) GLOBAL_UNCERTAINTY_ASSIGNED_CONTEXT ( ( #3583 ) ) GLOBAL_UNIT_ASSIGNED_CONTEXT ( ( #4188, #675, #6404 ) ) REPRESENTATION_CONTEXT ( 'NONE', 'WORKASPACE' ) );
#7345 = CARTESIAN_POINT ( 'NONE',  ( 0.2371576072764298437, -0.2722228516542264942, -0.003016182236739480948 ) ) ;
#7346 = ORIENTED_EDGE ( 'NONE', *, *, #1863, .F. ) ;
#7347 = DIRECTION ( 'NONE',  ( -0.000000000000000000, -0.000000000000000000, 1.000000000000000000 ) ) ;
#7348 = ORIENTED_EDGE ( 'NONE', *, *, #3270, .F. ) ;
#7349 = CARTESIAN_POINT ( 'NONE',  ( 1.611653543307086212, 2.892866454678787531E-17, -0.2362204724409449064 ) ) ;
#7350 = ORIENTED_EDGE ( 'NONE', *, *, #7241, .F. ) ;
#7351 =( NAMED_UNIT ( * ) PLANE_ANGLE_UNIT ( ) SI_UNIT ( $, .RADIAN. ) );
#7352 = ORIENTED_EDGE ( 'NONE', *, *, #664, .T. ) ;
#7353 = AXIS2_PLACEMENT_3D ( 'NONE', #3580, #3433, #102 ) ;
#7354 = CARTESIAN_POINT ( 'NONE',  ( 1.968503937007874072, 1.205361022782827973E-16, -0.9842519685039370358 ) ) ;
#7355 = DIRECTION ( 'NONE',  ( 0.8672889550420767035, -0.4978050506594153823, 1.030029033886335351E-15 ) ) ;
#7356 = CARTESIAN_POINT ( 'NONE',  ( 0.000000000000000000, 0.000000000000000000, 0.000000000000000000 ) ) ;
#7357 = CARTESIAN_POINT ( 'NONE',  ( 1.045446081760740942, -0.2286795840550674142, -0.9573229298165720769 ) ) ;
#7358 = AXIS2_PLACEMENT_3D ( 'NONE', #3478, #5815, #1744 ) ;
#7359 = DIRECTION ( 'NONE',  ( -0.000000000000000000, -0.000000000000000000, 1.000000000000000000 ) ) ;
#7360 = FACE_OUTER_BOUND ( 'NONE', #7230, .T. ) ;
#7361 = CARTESIAN_POINT ( 'NONE',  ( 0.3581828924050323715, 0.1743168766271107895, -0.3019256869348722061 ) ) ;
#7362 = CYLINDRICAL_SURFACE ( 'NONE', #7414, 0.2362204724409449064 ) ;
#7363 = ORIENTED_EDGE ( 'NONE', *, *, #2754, .F. ) ;
#7364 = FACE_OUTER_BOUND ( 'NONE', #6391, .T. ) ;
#7365 = VECTOR ( 'NONE', #6302, 39.37007874015748143 ) ;
#7366 = ORIENTED_EDGE ( 'NONE', *, *, #4303, .F. ) ;
#7367 = CARTESIAN_POINT ( 'NONE',  ( 0.3527006543068523237, 0.1709223289430787940, -0.2960461578774135072 ) ) ;
#7368 = DIRECTION ( 'NONE',  ( -0.000000000000000000, -0.000000000000000000, -1.000000000000000000 ) ) ;
#7369 = CLOSED_SHELL ( 'NONE', ( #2168, #6598, #7193, #2805, #1425, #4963, #4066, #5002, #1189 ) ) ;
#7370 = CARTESIAN_POINT ( 'NONE',  ( 0.5141614760841457521, 0.000000000000000000, -2.204724409448820754 ) ) ;
#7371 = ORIENTED_EDGE ( 'NONE', *, *, #2989, .T. ) ;
#7372 = CARTESIAN_POINT ( 'NONE',  ( 0.1771653543307089296, -0.3068593950417301541, -0.4082677165354330340 ) ) ;
#7373 = CARTESIAN_POINT ( 'NONE',  ( 0.3565422270302655572, 0.1673297761639317704, -0.3007275071673040645 ) ) ;
#7374 = ADVANCED_FACE ( 'NONE', ( #1125 ), #7022, .F. ) ;
#7375 = EDGE_CURVE ( 'NONE', #4992, #670, #6978, .T. ) ;
#7376 = VERTEX_POINT ( 'NONE', #4153 ) ;
#7377 = ORIENTED_EDGE ( 'NONE', *, *, #5162, .F. ) ;
#7378 = EDGE_CURVE ( 'NONE', #1597, #7376, #5876, .T. ) ;
#7379 = DIRECTION ( 'NONE',  ( -0.000000000000000000, -1.000000000000000000, -0.000000000000000000 ) ) ;
#7380 = CARTESIAN_POINT ( 'NONE',  ( 0.3528850351813199171, 0.3340780101605773655, 0.02497973507596915402 ) ) ;
#7381 =( NAMED_UNIT ( * ) SI_UNIT ( $, .STERADIAN. ) SOLID_ANGLE_UNIT ( ) );
#7382 = EDGE_LOOP ( 'NONE', ( #4209, #21, #1573, #2553 ) ) ;
#7383 = CARTESIAN_POINT ( 'NONE',  ( 0.3391892065151629332, -0.1988903486381584651, 0.2460629921259843145 ) ) ;
#7384 = ORIENTED_EDGE ( 'NONE', *, *, #1880, .T. ) ;
#7385 = CARTESIAN_POINT ( 'NONE',  ( 0.9479499796399277756, 0.4353079511162336046, -1.456692913385828625 ) ) ;
#7386 = B_SPLINE_CURVE_WITH_KNOTS ( 'NONE', 3,
 ( #2574, #4911, #1416, #6674, #3802, #405 ),
 .UNSPECIFIED., .F., .F.,
 ( 4, 2, 4 ),
 ( 0.009270618776430216562, 0.01189894710419331023, 0.01452727543195640389 ),
 .UNSPECIFIED. ) ;
#7387 = EDGE_CURVE ( 'NONE', #4527, #3346, #6127, .T. ) ;
#7388 = EDGE_LOOP ( 'NONE', ( #843, #3805, #2192, #7491 ) ) ;
#7389 = EDGE_CURVE ( 'NONE', #698, #2401, #4954, .T. ) ;
#7390 = CARTESIAN_POINT ( 'NONE',  ( 0.3398312250857989381, 0.3151631602416481437, 0.04467257488985636182 ) ) ;
#7391 = EDGE_LOOP ( 'NONE', ( #5333, #1185, #4378 ) ) ;
#7392 = CARTESIAN_POINT ( 'NONE',  ( 0.000000000000000000, 2.892866454678787531E-17, -0.2362204724409449064 ) ) ;
#7393 = DIRECTION ( 'NONE',  ( -4.151318482771456951E-16, 1.972152263052529514E-31, 1.000000000000000000 ) ) ;
#7394 = CARTESIAN_POINT ( 'NONE',  ( 0.3581828924050324825, -0.1743168766271116221, -0.3019256869348722061 ) ) ;
#7395 = CARTESIAN_POINT ( 'NONE',  ( 0.9346850374427910779, 0.4388996395293667807, -1.455943645409048637 ) ) ;
#7396 = B_SPLINE_CURVE_WITH_KNOTS ( 'NONE', 3,
 ( #7260, #6661, #3828, #2033, #1515, #4361 ),
 .UNSPECIFIED., .F., .F.,
 ( 4, 2, 4 ),
 ( 0.02625214965902978106, 0.02844383079405753134, 0.03063551192908527815 ),
 .UNSPECIFIED. ) ;
#7397 = FACE_OUTER_BOUND ( 'NONE', #2889, .T. ) ;
#7398 = CARTESIAN_POINT ( 'NONE',  ( 0.8865586066401955900, 0.2152123167378564572, -0.9604399500593175931 ) ) ;
#7399 = EDGE_LOOP ( 'NONE', ( #3177, #1619 ) ) ;
#7400 = CARTESIAN_POINT ( 'NONE',  ( 0.002513486811083624848, -0.2845799557467911245, 0.09764423893321799719 ) ) ;
#7401 = CARTESIAN_POINT ( 'NONE',  ( 0.3459463601587710602, -0.3157502742997210787, 0.04365566351110977683 ) ) ;
#7402 = CARTESIAN_POINT ( 'NONE',  ( -0.4663806185492885836, -0.8833138556570210298, -1.436938405272246921 ) ) ;
#7403 = CARTESIAN_POINT ( 'NONE',  ( -0.4700904924197902846, 0.9659644734970543878, -1.546597720061111847 ) ) ;
#7404 = B_SPLINE_CURVE_WITH_KNOTS ( 'NONE', 3,
 ( #5584, #4536, #3969, #4577, #6297, #5733, #6906, #6152 ),
 .UNSPECIFIED., .F., .F.,
 ( 4, 2, 2, 4 ),
 ( 0.004381617662950723809, 0.005472867551409551883, 0.006564117439868379089, 0.008746617216786035237 ),
 .UNSPECIFIED. ) ;
#7405 = ORIENTED_EDGE ( 'NONE', *, *, #3232, .T. ) ;
#7406 = DIRECTION ( 'NONE',  ( 0.000000000000000000, 0.000000000000000000, -1.000000000000000000 ) ) ;
#7407 = CARTESIAN_POINT ( 'NONE',  ( 0.2520187439128737106, 0.2636427704167111918, -0.4024809188492816658 ) ) ;
#7408 = CONTEXT_DEPENDENT_SHAPE_REPRESENTATION ( #6385, #6735 ) ;
#7409 = CARTESIAN_POINT ( 'NONE',  ( -0.3543307086614173040, -0.2045729300278205653, -0.4082677165354330340 ) ) ;
#7410 = ORIENTED_EDGE ( 'NONE', *, *, #5791, .F. ) ;
#7411 = CARTESIAN_POINT ( 'NONE',  ( 1.055789886223273654E-16, -0.2411939993270979798, -0.1727909197870958757 ) ) ;
#7412 = CARTESIAN_POINT ( 'NONE',  ( 0.3403864257300893703, -0.2263128404110642256, 0.1985658431051765538 ) ) ;
#7413 = EDGE_LOOP ( 'NONE', ( #7155, #5329, #6687, #6969, #6931, #7327, #514, #172, #2448, #519, #3835, #7299 ) ) ;
#7414 = AXIS2_PLACEMENT_3D ( 'NONE', #4544, #6229, #2814 ) ;
#7415 = ORIENTED_EDGE ( 'NONE', *, *, #2934, .T. ) ;
#7416 = CARTESIAN_POINT ( 'NONE',  ( -1.718248690375557255E-15, 0.4921259842519683514, -2.204724409448820754 ) ) ;
#7417 = CARTESIAN_POINT ( 'NONE',  ( -1.781909941321919274E-15, 0.000000000000000000, -1.397637795275591843 ) ) ;
#7418 = EDGE_CURVE ( 'NONE', #6357, #1871, #5701, .T. ) ;
#7419 = DIRECTION ( 'NONE',  ( 1.224646799147353207E-16, 1.000000000000000000, 0.000000000000000000 ) ) ;
#7420 = VERTEX_POINT ( 'NONE', #3237 ) ;
#7421 = DIRECTION ( 'NONE',  ( 1.000000000000000000, 0.000000000000000000, -0.000000000000000000 ) ) ;
#7422 = ORIENTED_EDGE ( 'NONE', *, *, #7152, .T. ) ;
#7423 = AXIS2_PLACEMENT_3D ( 'NONE', #928, #6785, #4986 ) ;
#7424 = CARTESIAN_POINT ( 'NONE',  ( 0.3322361761492683696, 0.2247851515112334331, 0.2012118778978378431 ) ) ;
#7425 = ORIENTED_EDGE ( 'NONE', *, *, #6405, .T. ) ;
#7426 = ORIENTED_EDGE ( 'NONE', *, *, #6306, .F. ) ;
#7427 = ADVANCED_FACE ( 'NONE', ( #3738 ), #306, .F. ) ;
#7428 = EDGE_CURVE ( 'NONE', #5941, #6730, #4540, .T. ) ;
#7429 = CARTESIAN_POINT ( 'NONE',  ( 18.41860179314716817, 41.48855051017370243, 52.63397348499201200 ) ) ;
#7430 = CARTESIAN_POINT ( 'NONE',  ( 0.8884031170519930409, 0.4627498550472279870, -1.439912866901233990 ) ) ;
#7431 = CARTESIAN_POINT ( 'NONE',  ( 3.027559055118110187, 0.000000000000000000, 0.000000000000000000 ) ) ;
#7432 = EDGE_CURVE ( 'NONE', #772, #6852, #909, .T. ) ;
#7433 = AXIS2_PLACEMENT_3D ( 'NONE', #4320, #6653, #3744 ) ;
#7434 = DIRECTION ( 'NONE',  ( -0.000000000000000000, 0.000000000000000000, -1.000000000000000000 ) ) ;
#7435 = DIRECTION ( 'NONE',  ( -1.000000000000000000, 0.000000000000000000, 0.000000000000000000 ) ) ;
#7436 = AXIS2_PLACEMENT_3D ( 'NONE', #4273, #5390, #2549 ) ;
#7437 = PLANE ( 'NONE',  #4451 ) ;
#7438 = CARTESIAN_POINT ( 'NONE',  ( 0.3585569128062321420, -0.3496569568119795024, -0.001755940978325754281 ) ) ;
#7439 = FACE_OUTER_BOUND ( 'NONE', #3907, .T. ) ;
#7440 = CARTESIAN_POINT ( 'NONE',  ( 0.3410249605999410294, -1.062517223525361548E-12, -0.3014927230551905368 ) ) ;
#7441 = AXIS2_PLACEMENT_3D ( 'NONE', #4235, #5926, #2393 ) ;
#7442 = EDGE_LOOP ( 'NONE', ( #6281, #2149, #612, #2904 ) ) ;
#7443 = CARTESIAN_POINT ( 'NONE',  ( 0.4349192646538860285, -0.9810555383103363170, -1.448591292758282023 ) ) ;
#7444 = CARTESIAN_POINT ( 'NONE',  ( 0.1771653543307089296, 0.3068593950417301541, -0.4082677165354330340 ) ) ;
#7445 = CARTESIAN_POINT ( 'NONE',  ( 0.3483227611829848303, -0.1704774416898505729, -0.2952755905511810774 ) ) ;
#7446 = VERTEX_POINT ( 'NONE', #3161 ) ;
#7447 = CARTESIAN_POINT ( 'NONE',  ( 0.3510872220067887683, 0.1819230426404221390, -0.2754512281816320352 ) ) ;
#7448 = CYLINDRICAL_SURFACE ( 'NONE', #889, 0.2066929133858267931 ) ;
#7449 = APPLICATION_CONTEXT ( 'automotive_design' ) ;
#7450 = VERTEX_POINT ( 'NONE', #5508 ) ;
#7451 = AXIS2_PLACEMENT_3D ( 'NONE', #4299, #3732, #4342 ) ;
#7452 = ORIENTED_EDGE ( 'NONE', *, *, #1154, .T. ) ;
#7453 = CARTESIAN_POINT ( 'NONE',  ( 1.189177986357916605, -0.1185041968903534776, 0.9771775582510943137 ) ) ;
#7454 = CARTESIAN_POINT ( 'NONE',  ( 0.000000000000000000, 1.496062992125984259, 0.000000000000000000 ) ) ;
#7455 =( NAMED_UNIT ( * ) PLANE_ANGLE_UNIT ( ) SI_UNIT ( $, .RADIAN. ) );
#7456 = ORIENTED_EDGE ( 'NONE', *, *, #7432, .F. ) ;
#7457 = CARTESIAN_POINT ( 'NONE',  ( -2.403706095987794643E-16, 0.2484822268960368286, -0.1601673393405684265 ) ) ;
#7458 = ORIENTED_EDGE ( 'NONE', *, *, #4398, .T. ) ;
#7459 = CIRCLE ( 'NONE', #2580, 0.05905511811023620578 ) ;
#7460 = DIRECTION ( 'NONE',  ( -1.000000000000000000, -0.000000000000000000, 0.000000000000000000 ) ) ;
#7461 = EDGE_CURVE ( 'NONE', #283, #269, #4782, .T. ) ;
#7462 = VERTEX_POINT ( 'NONE', #7281 ) ;
#7463 = AXIS2_PLACEMENT_3D ( 'NONE', #3931, #7434, #3890 ) ;
#7464 = PLANE ( 'NONE',  #669 ) ;
#7465 = DIRECTION ( 'NONE',  ( -2.320548612096681119E-16, 8.648785545355717899E-18, 1.000000000000000000 ) ) ;
#7466 = CIRCLE ( 'NONE', #1853, 0.9842519685039370358 ) ;
#7467 = FACE_OUTER_BOUND ( 'NONE', #4659, .T. ) ;
#7468 = AXIS2_PLACEMENT_3D ( 'NONE', #551, #7460, #1616 ) ;
#7469 = FACE_BOUND ( 'NONE', #4184, .T. ) ;
#7470 = ADVANCED_FACE ( 'NONE', ( #7208 ), #263, .F. ) ;
#7471 = ADVANCED_FACE ( 'NONE', ( #6112 ), #2586, .F. ) ;
#7472 = EDGE_CURVE ( 'NONE', #4759, #5905, #1938, .T. ) ;
#7473 = VECTOR ( 'NONE', #3249, 39.37007874015748143 ) ;
#7474 = CARTESIAN_POINT ( 'NONE',  ( 0.9221073153504563136, -0.4437903857718229483, -1.453484209829403850 ) ) ;
#7475 = PLANE ( 'NONE',  #4679 ) ;
#7476 = CARTESIAN_POINT ( 'NONE',  ( -0.4921259842519648542, 0.000000000000000000, -2.204724409448822975 ) ) ;
#7477 = UNCERTAINTY_MEASURE_WITH_UNIT (LENGTH_MEASURE( 1.000000000000000082E-05 ), #4575, 'distance_accuracy_value', 'NONE');
#7478 = CARTESIAN_POINT ( 'NONE',  ( 3.027559055118110187, 0.000000000000000000, 0.1982677165354330695 ) ) ;
#7479 = ADVANCED_FACE ( 'NONE', ( #226, #4843 ), #6003, .F. ) ;
#7480 = CONICAL_SURFACE ( 'NONE', #1472, 0.2952755905511810774, 1.047197551196600518 ) ;
#7481 = DIRECTION ( 'NONE',  ( 0.000000000000000000, -0.000000000000000000, 1.000000000000000000 ) ) ;
#7482 = CARTESIAN_POINT ( 'NONE',  ( 0.2962704110120346623, 0.2380940585049209357, -0.3942118233966399599 ) ) ;
#7483 = ITEM_DEFINED_TRANSFORMATION ( 'NONE', 'NONE', #1286,  #5166 ) ;
#7484 = CARTESIAN_POINT ( 'NONE',  ( -0.9941399105654876722, -0.4762522394722520369, -1.397361772547374814 ) ) ;
#7485 = ORIENTED_EDGE ( 'NONE', *, *, #4860, .T. ) ;
#7486 = CARTESIAN_POINT ( 'NONE',  ( 0.3496779274129792059, 0.3447056852546006578, 0.006496579416451838881 ) ) ;
#7487 = DIRECTION ( 'NONE',  ( 0.000000000000000000, -1.000000000000000000, 0.000000000000000000 ) ) ;
#7488 = VERTEX_POINT ( 'NONE', #3816 ) ;
#7489 = ORIENTED_EDGE ( 'NONE', *, *, #6396, .T. ) ;
#7490 = CARTESIAN_POINT ( 'NONE',  ( 0.7794093496269024479, -0.1186414295356391785, 0.9771602695683655471 ) ) ;
#7491 = ORIENTED_EDGE ( 'NONE', *, *, #2066, .F. ) ;
#7492 = CARTESIAN_POINT ( 'NONE',  ( 0.3483227611829848303, -0.1704774416898505729, -0.2952755905511810774 ) ) ;
#7493 = ORIENTED_EDGE ( 'NONE', *, *, #4497, .T. ) ;
#7494 = CARTESIAN_POINT ( 'NONE',  ( 1.196402575039207328, 0.1050201062211118808, 0.9787371541722721391 ) ) ;
#7495 = CARTESIAN_POINT ( 'NONE',  ( 0.3410249605999410294, 1.062103031354818709E-12, 0.3014927230551906479 ) ) ;
#7496 = ORIENTED_EDGE ( 'NONE', *, *, #2250, .T. ) ;
#7497 = DIMENSIONAL_EXPONENTS ( 1.000000000000000000, 0.000000000000000000, 0.000000000000000000, 0.000000000000000000, 0.000000000000000000, 0.000000000000000000, 0.000000000000000000 ) ;
#7498 = VERTEX_POINT ( 'NONE', #6682 ) ;
#7499 = DIRECTION ( 'NONE',  ( -0.000000000000000000, -0.000000000000000000, 1.000000000000000000 ) ) ;
#7500 =( CONVERSION_BASED_UNIT ( 'INCH', #2841 ) LENGTH_UNIT ( ) NAMED_UNIT ( #6875 ) );
#7501 = CARTESIAN_POINT ( 'NONE',  ( 0.3527006543068526567, -0.3418446578861590868, 8.418741006566202135E-18 ) ) ;
#7502 = CARTESIAN_POINT ( 'NONE',  ( -0.1023119647485438433, 0.3500760196667492274, -0.4024809188492814993 ) ) ;
#7503 =( LENGTH_UNIT ( ) NAMED_UNIT ( * ) SI_UNIT ( $, .METRE. ) );
#7504 =( LENGTH_UNIT ( ) NAMED_UNIT ( * ) SI_UNIT ( $, .METRE. ) );
#7505 = EDGE_CURVE ( 'NONE', #2829, #2119, #6611, .T. ) ;
#7506 = CARTESIAN_POINT ( 'NONE',  ( 0.3410425348215777031, -0.2462961272004795532, -0.1763890642357578975 ) ) ;
#7507 = CARTESIAN_POINT ( 'NONE',  ( 0.5118110236220474452, 1.220472440944881942, 0.4724409448818898127 ) ) ;
#7508 = DIRECTION ( 'NONE',  ( 0.000000000000000000, 0.000000000000000000, -1.000000000000000000 ) ) ;
#7509 = EDGE_CURVE ( 'NONE', #3761, #4821, #2107, .T. ) ;
#7510 = CARTESIAN_POINT ( 'NONE',  ( -0.9159932075028757170, 0.4466261709646344169, -1.451746187131333521 ) ) ;
#7511 = LINE ( 'NONE', #4587, #627 ) ;
#7512 = CARTESIAN_POINT ( 'NONE',  ( 0.01168997831664865018, 0.3129651733100085598, -0.04847959992982851796 ) ) ;
#7513 = EDGE_CURVE ( 'NONE', #5534, #4463, #146, .T. ) ;
#7514 = EDGE_CURVE ( 'NONE', #5565, #5211, #2226, .T. ) ;
#7515 = CARTESIAN_POINT ( 'NONE',  ( 0.000000000000000000, 0.000000000000000000, 0.000000000000000000 ) ) ;
#7516 = ORIENTED_EDGE ( 'NONE', *, *, #6995, .F. ) ;
#7517 = CARTESIAN_POINT ( 'NONE',  ( 1.649606299212598381, 0.000000000000000000, 0.000000000000000000 ) ) ;
#7518 = EDGE_CURVE ( 'NONE', #1871, #630, #3311, .T. ) ;
#7519 = NEXT_ASSEMBLY_USAGE_OCCURRENCE ( 'NAUO1', ' ', ' ', #3831, #6029, $ ) ;
#7520 = NEXT_ASSEMBLY_USAGE_OCCURRENCE ( 'NAUO2', ' ', ' ', #3831, #1953, $ ) ;
#7521 = NEXT_ASSEMBLY_USAGE_OCCURRENCE ( 'NAUO3', ' ', ' ', #3831, #5928, $ ) ;
#7522 = NEXT_ASSEMBLY_USAGE_OCCURRENCE ( 'NAUO4', ' ', ' ', #3831, #2745, $ ) ;
#7523 = NEXT_ASSEMBLY_USAGE_OCCURRENCE ( 'NAUO5', ' ', ' ', #3831, #5662, $ ) ;
#7524 = NEXT_ASSEMBLY_USAGE_OCCURRENCE ( 'NAUO6', ' ', ' ', #3831, #2700, $ ) ;
#7525 = NEXT_ASSEMBLY_USAGE_OCCURRENCE ( 'NAUO7', ' ', ' ', #3831, #2745, $ ) ;
#7526 = NEXT_ASSEMBLY_USAGE_OCCURRENCE ( 'NAUO8', ' ', ' ', #3831, #2745, $ ) ;
#7527 = NEXT_ASSEMBLY_USAGE_OCCURRENCE ( 'NAUO9', ' ', ' ', #3831, #2745, $ ) ;
#7528 = NEXT_ASSEMBLY_USAGE_OCCURRENCE ( 'NAUO10', ' ', ' ', #3831, #5662, $ ) ;
#7529 = NEXT_ASSEMBLY_USAGE_OCCURRENCE ( 'NAUO11', ' ', ' ', #3831, #2745, $ ) ;
#7530 = NEXT_ASSEMBLY_USAGE_OCCURRENCE ( 'NAUO12', ' ', ' ', #3831, #2745, $ ) ;
#7531 = NEXT_ASSEMBLY_USAGE_OCCURRENCE ( 'NAUO13', ' ', ' ', #3831, #2745, $ ) ;
#7532 = NEXT_ASSEMBLY_USAGE_OCCURRENCE ( 'NAUO14', ' ', ' ', #3831, #2745, $ ) ;
#7533 = NEXT_ASSEMBLY_USAGE_OCCURRENCE ( 'NAUO15', ' ', ' ', #3831, #787, $ ) ;
#7534 = NEXT_ASSEMBLY_USAGE_OCCURRENCE ( 'NAUO16', ' ', ' ', #3831, #787, $ ) ;
#7535 = NEXT_ASSEMBLY_USAGE_OCCURRENCE ( 'NAUO17', ' ', ' ', #3831, #787, $ ) ;
#7536 = NEXT_ASSEMBLY_USAGE_OCCURRENCE ( 'NAUO18', ' ', ' ', #3831, #787, $ ) ;
#7537 = NEXT_ASSEMBLY_USAGE_OCCURRENCE ( 'NAUO19', ' ', ' ', #3831, #5982, $ ) ;
#7538 = NEXT_ASSEMBLY_USAGE_OCCURRENCE ( 'NAUO20', ' ', ' ', #3831, #5982, $ ) ;
#7539 = NEXT_ASSEMBLY_USAGE_OCCURRENCE ( 'NAUO21', ' ', ' ', #3831, #5982, $ ) ;
#7540 = NEXT_ASSEMBLY_USAGE_OCCURRENCE ( 'NAUO22', ' ', ' ', #3831, #5982, $ ) ;
#7541 = NEXT_ASSEMBLY_USAGE_OCCURRENCE ( 'NAUO23', ' ', ' ', #3831, #5982, $ ) ;
#7542 = NEXT_ASSEMBLY_USAGE_OCCURRENCE ( 'NAUO24', ' ', ' ', #3831, #5982, $ ) ;
#7543 = NEXT_ASSEMBLY_USAGE_OCCURRENCE ( 'NAUO25', ' ', ' ', #3831, #558, $ ) ;
#7544 = NEXT_ASSEMBLY_USAGE_OCCURRENCE ( 'NAUO26', ' ', ' ', #3831, #558, $ ) ;
#7545 = NEXT_ASSEMBLY_USAGE_OCCURRENCE ( 'NAUO27', ' ', ' ', #3831, #558, $ ) ;
#7546 = NEXT_ASSEMBLY_USAGE_OCCURRENCE ( 'NAUO28', ' ', ' ', #3831, #558, $ ) ;
#7547 = NEXT_ASSEMBLY_USAGE_OCCURRENCE ( 'NAUO29', ' ', ' ', #3831, #558, $ ) ;
#7548 = NEXT_ASSEMBLY_USAGE_OCCURRENCE ( 'NAUO30', ' ', ' ', #3831, #558, $ ) ;
#7549 = NEXT_ASSEMBLY_USAGE_OCCURRENCE ( 'NAUO31', ' ', ' ', #3831, #558, $ ) ;
#7550 = NEXT_ASSEMBLY_USAGE_OCCURRENCE ( 'NAUO32', ' ', ' ', #3831, #558, $ ) ;
#7551 = NEXT_ASSEMBLY_USAGE_OCCURRENCE ( 'NAUO33', ' ', ' ', #3831, #558, $ ) ;
#7552 = NEXT_ASSEMBLY_USAGE_OCCURRENCE ( 'NAUO34', ' ', ' ', #3831, #558, $ ) ;
#7553=COLOUR_RGB('Dark Blue',0.08,0.2,0.34);
#7554=FILL_AREA_STYLE_COLOUR('',#7553);
#7555=FILL_AREA_STYLE('',(#7554));
#7556=SURFACE_STYLE_FILL_AREA(#7555);
#7557=SURFACE_SIDE_STYLE('',(#7556));
#7558=SURFACE_STYLE_USAGE(.BOTH.,#7557);
#7559=PRESENTATION_STYLE_ASSIGNMENT((#7558));
#7560=COLOUR_RGB('Light Blue',0.38,0.62,0.78);
#7561=FILL_AREA_STYLE_COLOUR('',#7560);
#7562=FILL_AREA_STYLE('',(#7561));
#7563=SURFACE_STYLE_FILL_AREA(#7562);
#7564=SURFACE_SIDE_STYLE('',(#7563));
#7565=SURFACE_STYLE_USAGE(.BOTH.,#7564);
#7566=PRESENTATION_STYLE_ASSIGNMENT((#7565));
#7567=COLOUR_RGB('Sky Blue',0.24,0.69,0.87);
#7568=FILL_AREA_STYLE_COLOUR('',#7567);
#7569=FILL_AREA_STYLE('',(#7568));
#7570=SURFACE_STYLE_FILL_AREA(#7569);
#7571=SURFACE_SIDE_STYLE('',(#7570));
#7572=SURFACE_STYLE_USAGE(.BOTH.,#7571);
#7573=PRESENTATION_STYLE_ASSIGNMENT((#7572));
#7574=COLOUR_RGB('Grey',0.48,0.52,0.57);
#7575=FILL_AREA_STYLE_COLOUR('',#7574);
#7576=FILL_AREA_STYLE('',(#7575));
#7577=SURFACE_STYLE_FILL_AREA(#7576);
#7578=SURFACE_SIDE_STYLE('',(#7577));
#7579=SURFACE_STYLE_USAGE(.BOTH.,#7578);
#7580=PRESENTATION_STYLE_ASSIGNMENT((#7579));
#7581=COLOUR_RGB('Black',0.12,0.14,0.17);
#7582=FILL_AREA_STYLE_COLOUR('',#7581);
#7583=FILL_AREA_STYLE('',(#7582));
#7584=SURFACE_STYLE_FILL_AREA(#7583);
#7585=SURFACE_SIDE_STYLE('',(#7584));
#7586=SURFACE_STYLE_USAGE(.BOTH.,#7585);
#7587=PRESENTATION_STYLE_ASSIGNMENT((#7586));
#7588=COLOUR_RGB('Off White',0.89,0.88,0.83);
#7589=FILL_AREA_STYLE_COLOUR('',#7588);
#7590=FILL_AREA_STYLE('',(#7589));
#7591=SURFACE_STYLE_FILL_AREA(#7590);
#7592=SURFACE_SIDE_STYLE('',(#7591));
#7593=SURFACE_STYLE_USAGE(.BOTH.,#7592);
#7594=PRESENTATION_STYLE_ASSIGNMENT((#7593));
ENDSEC;
END-ISO-10303-21;
